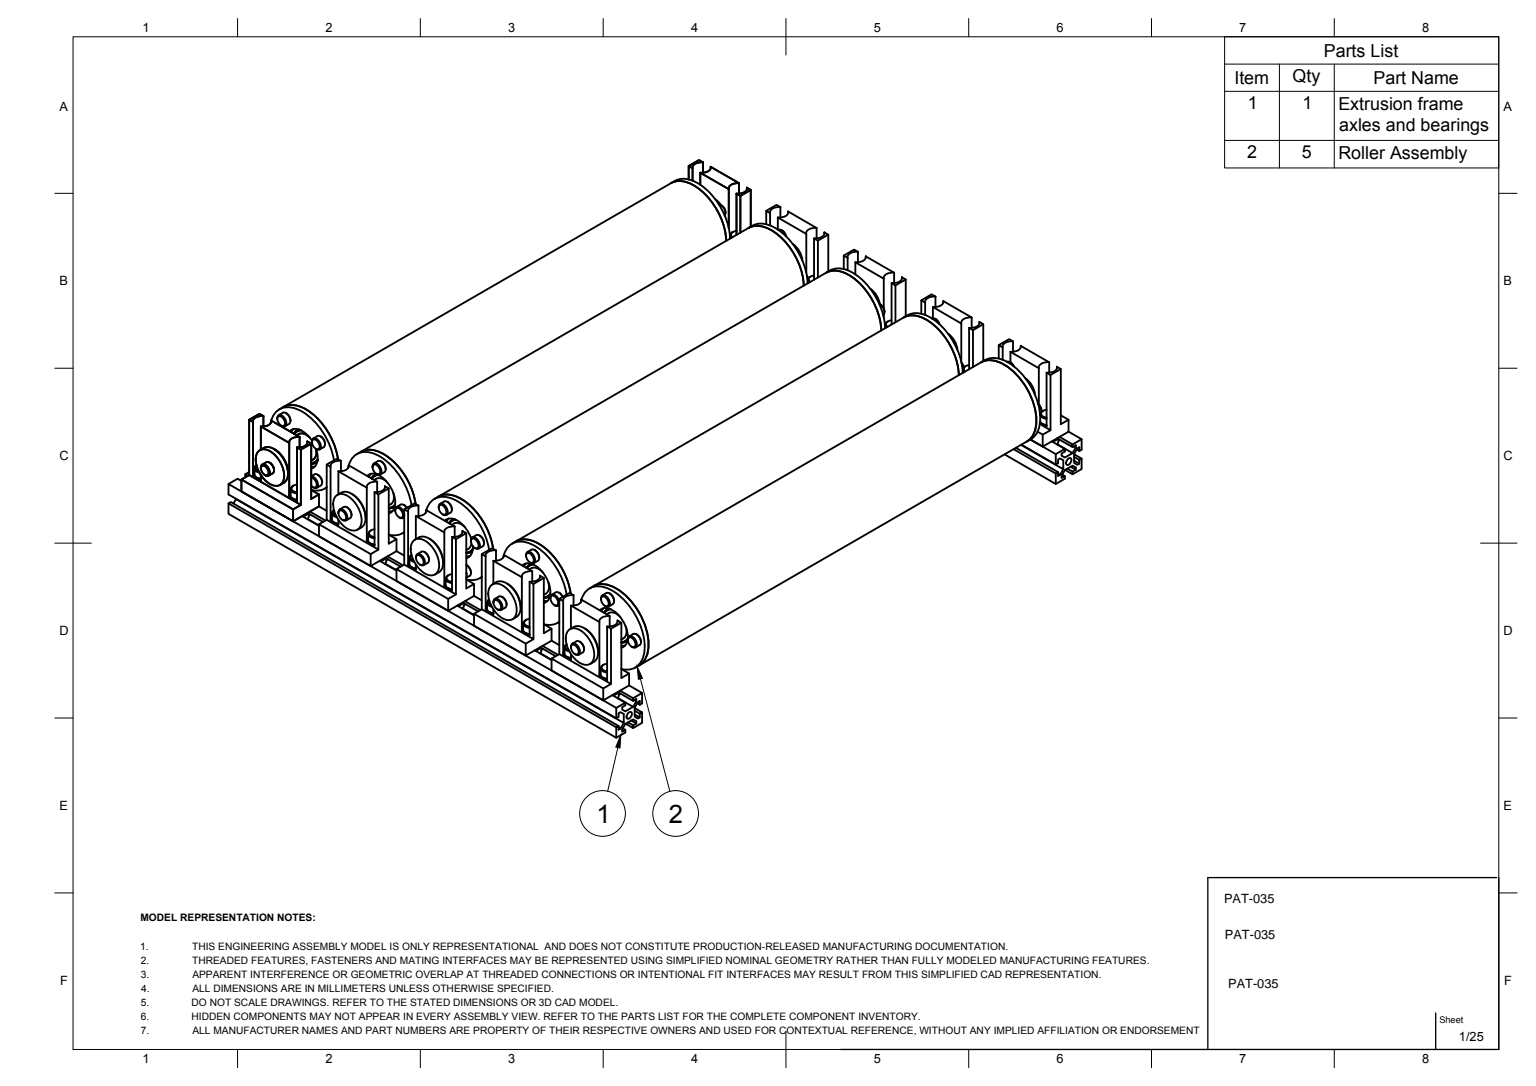
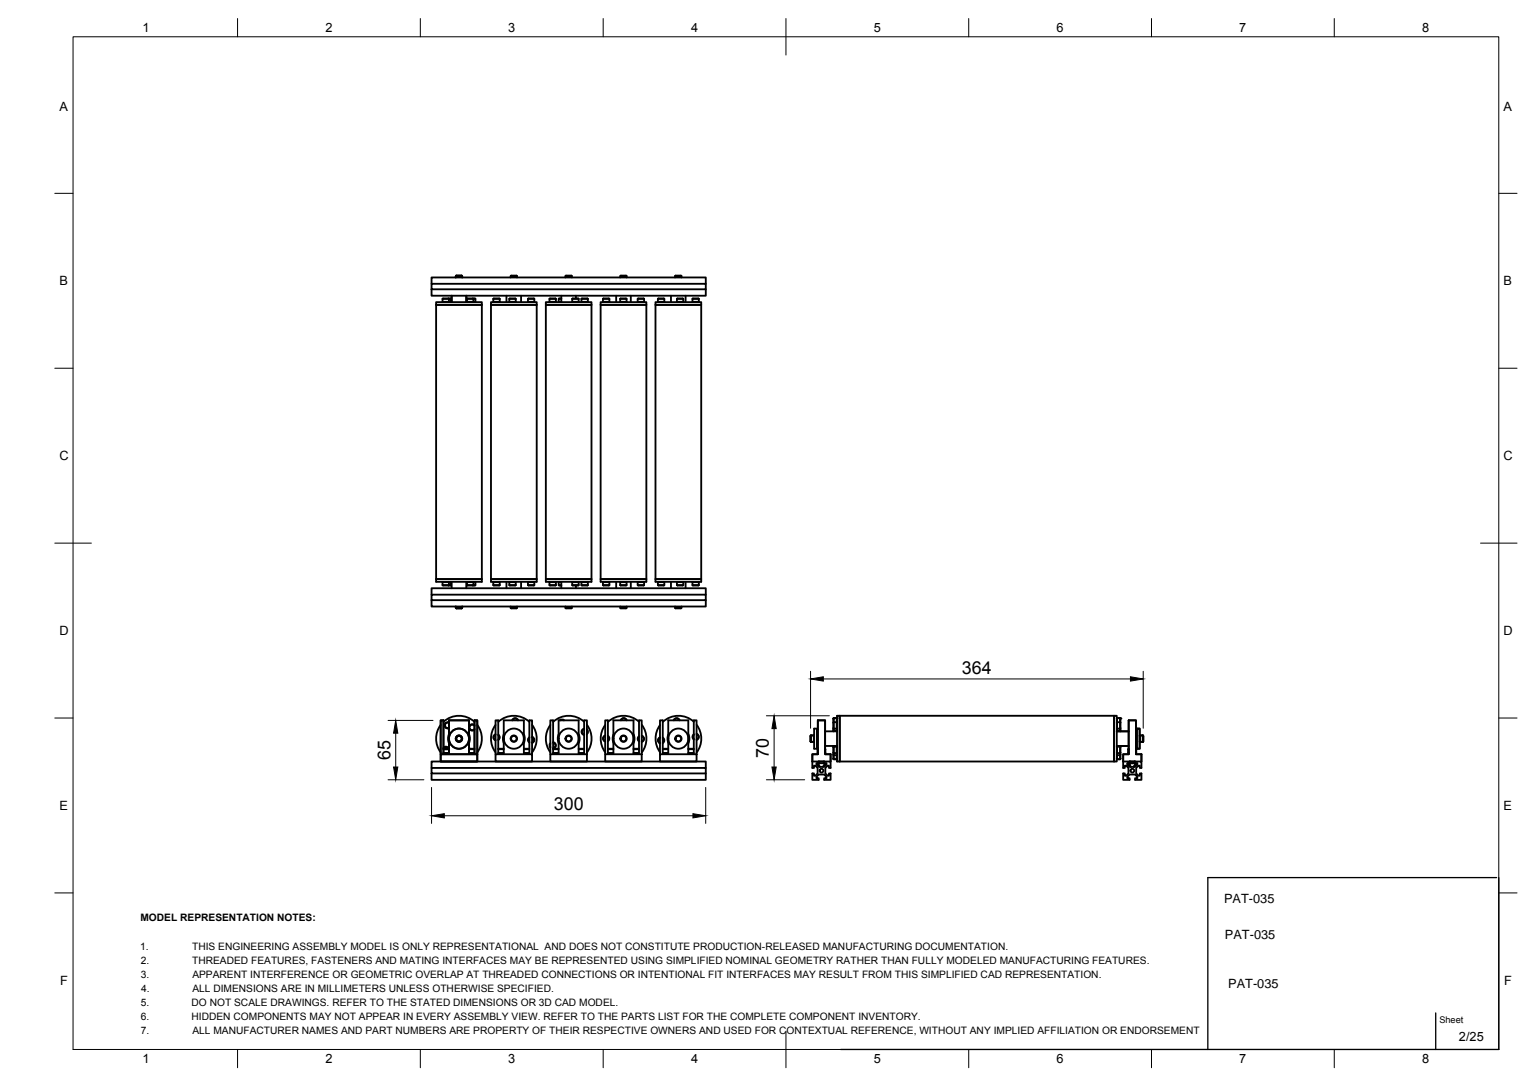
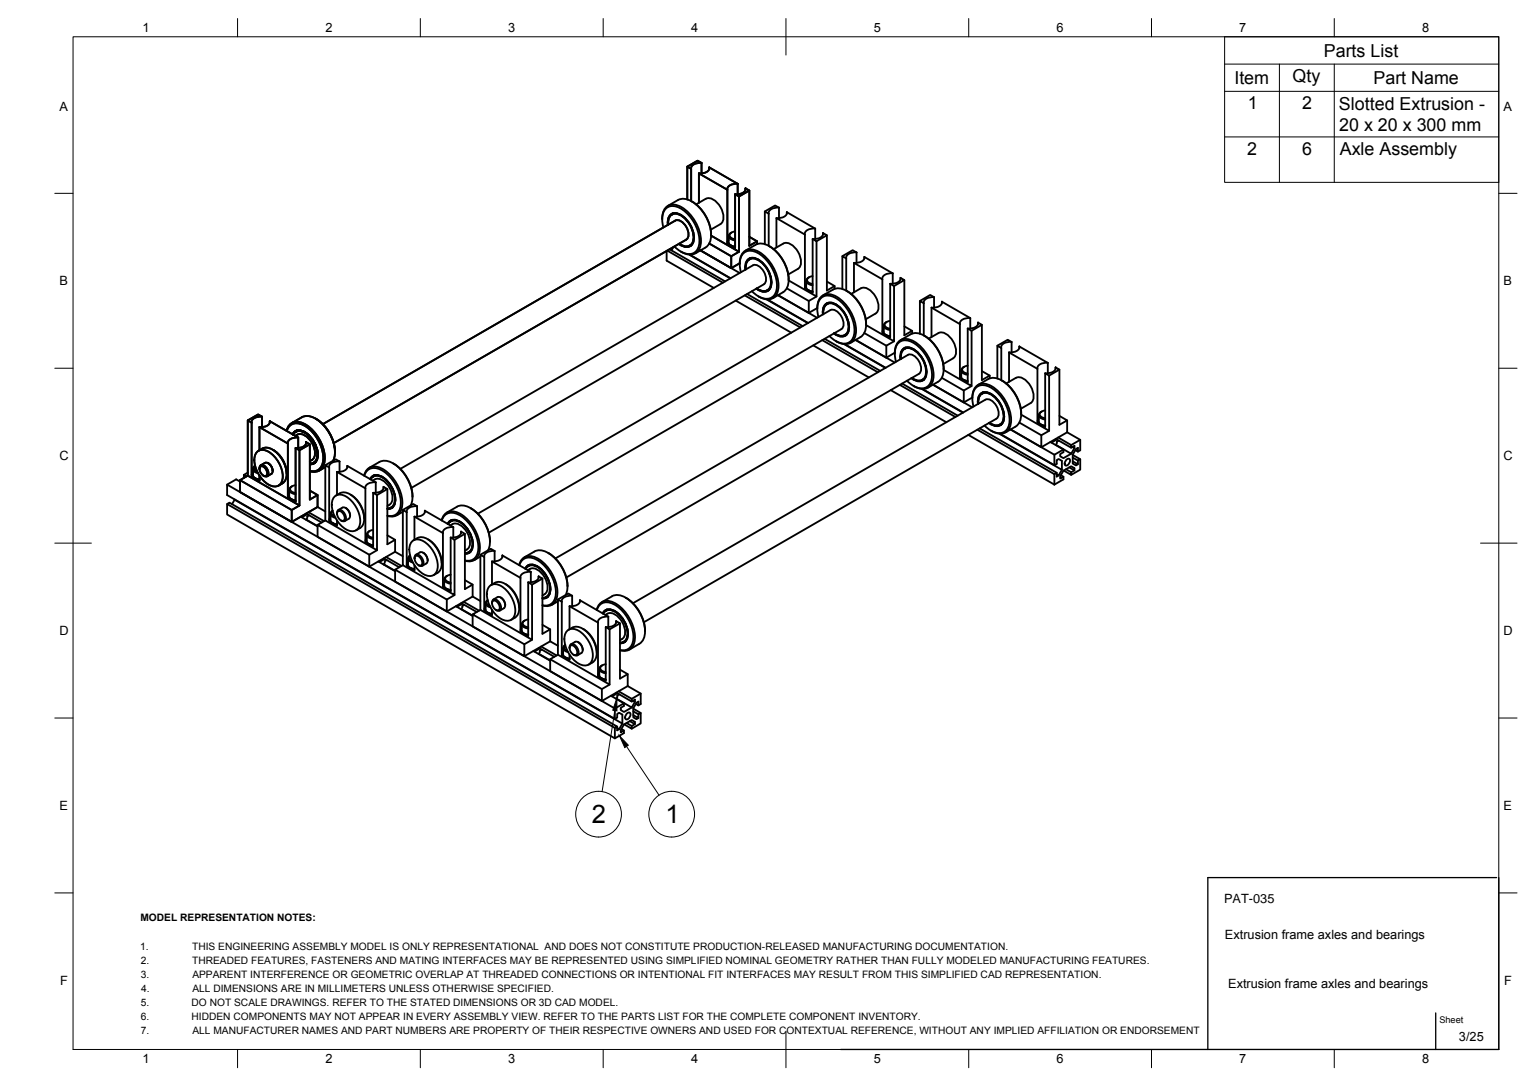
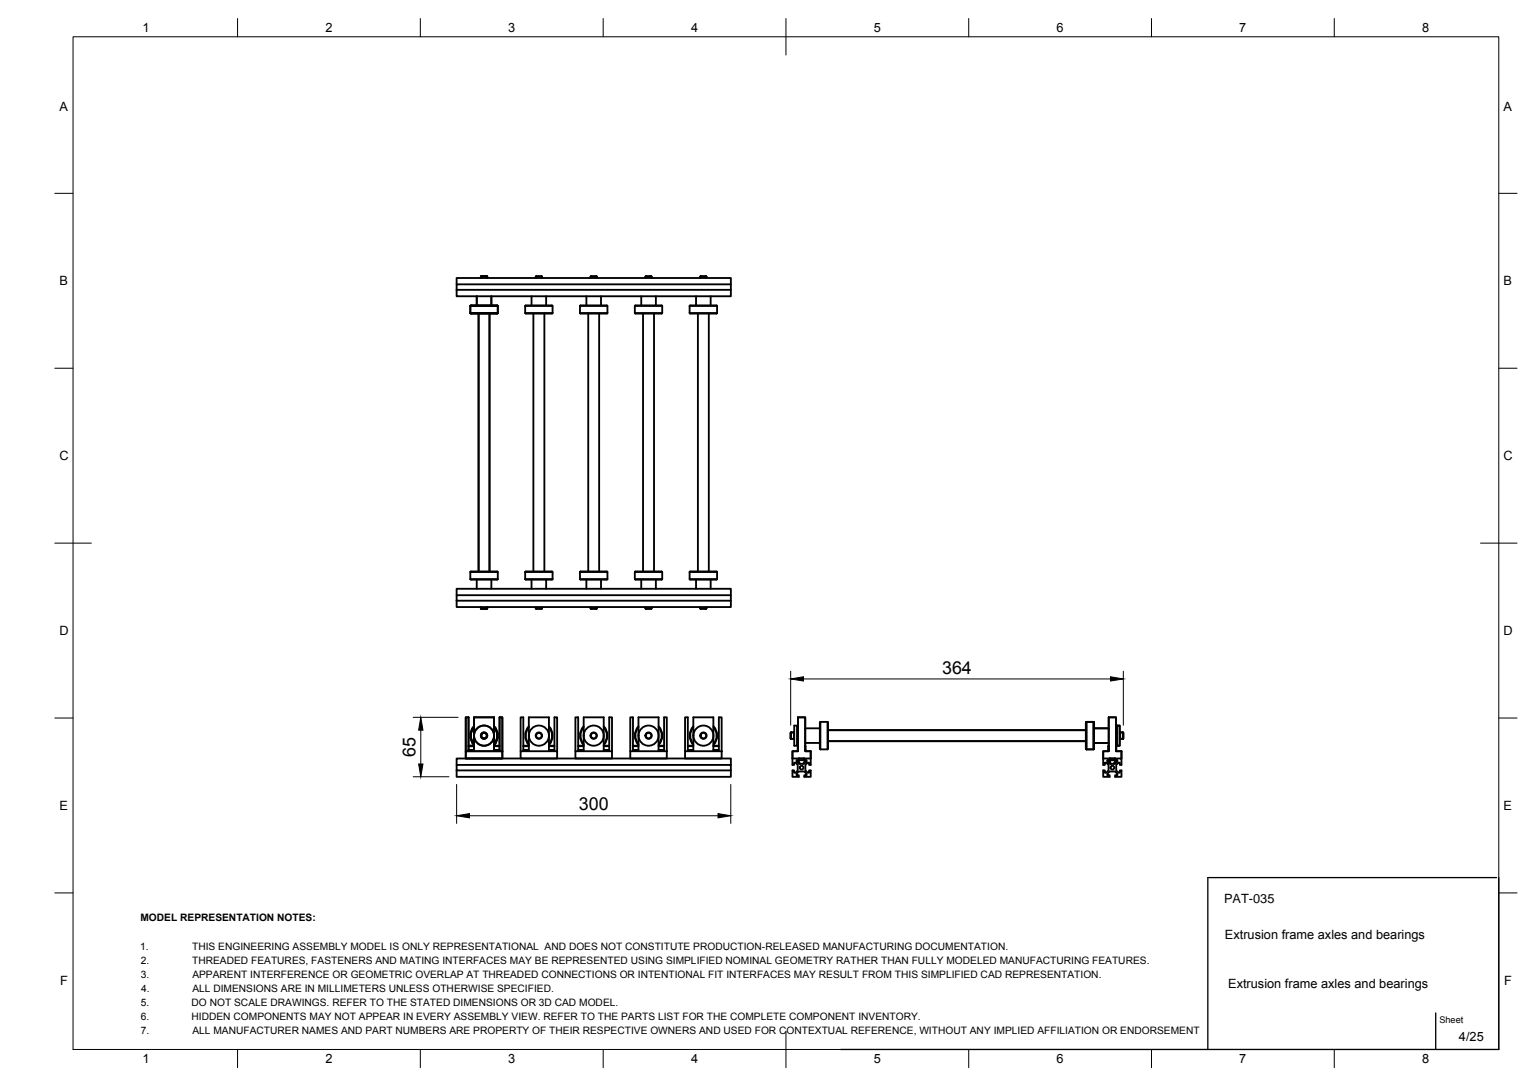
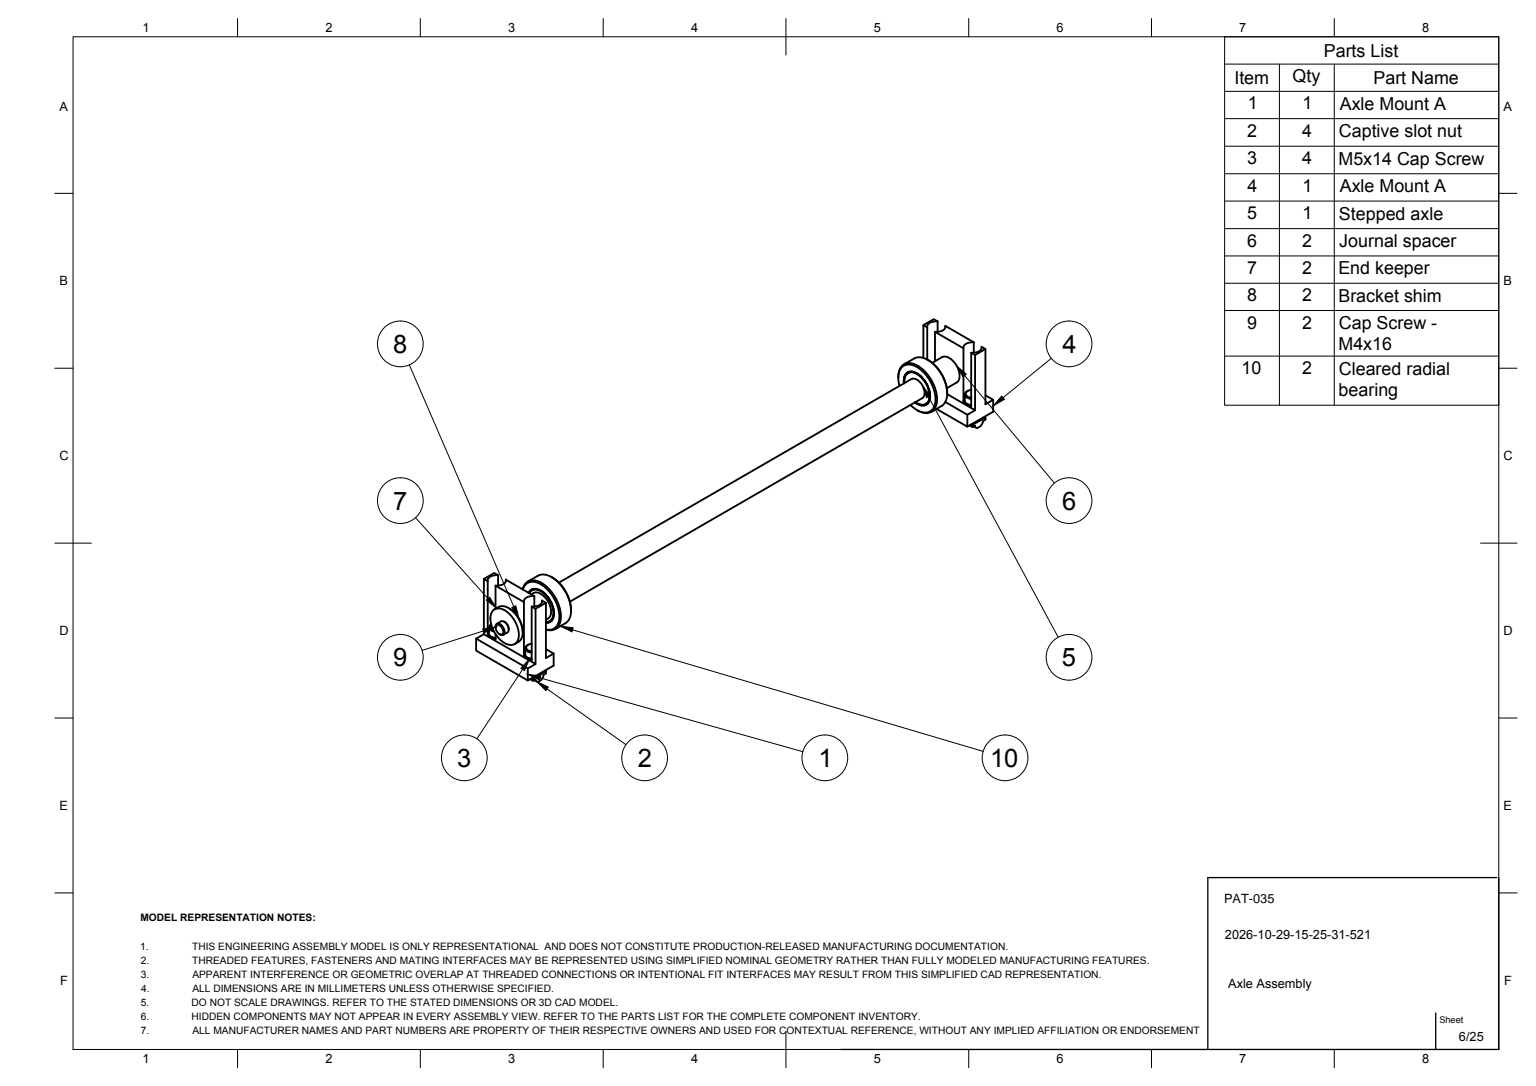
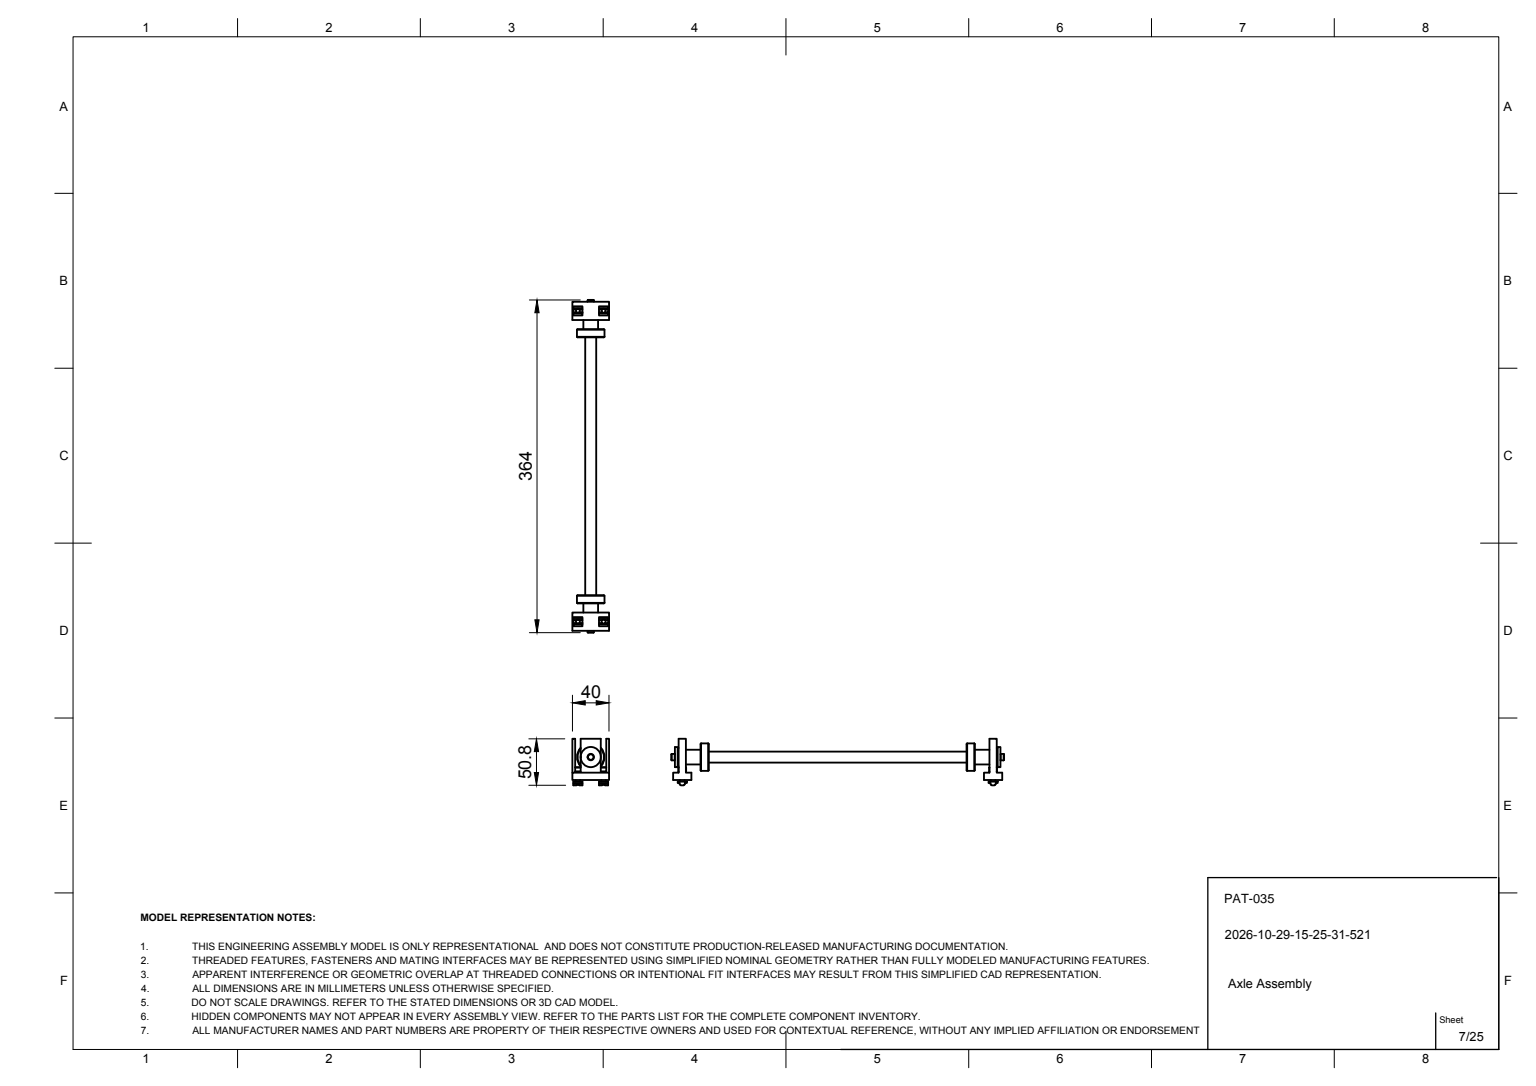
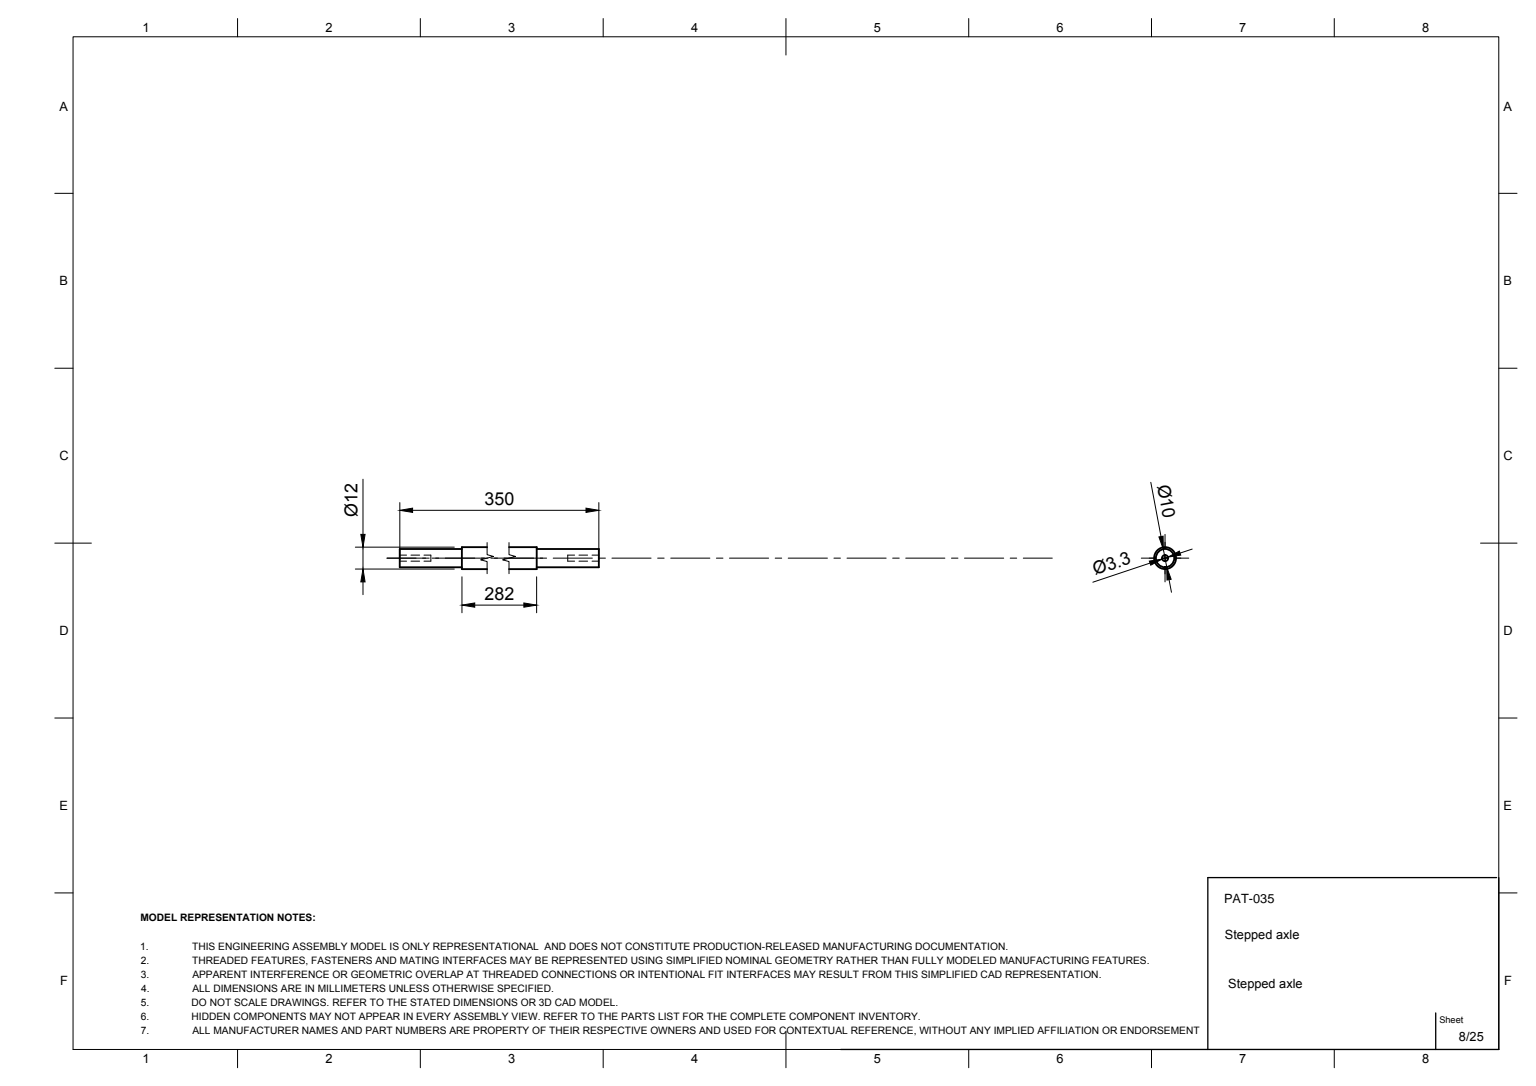
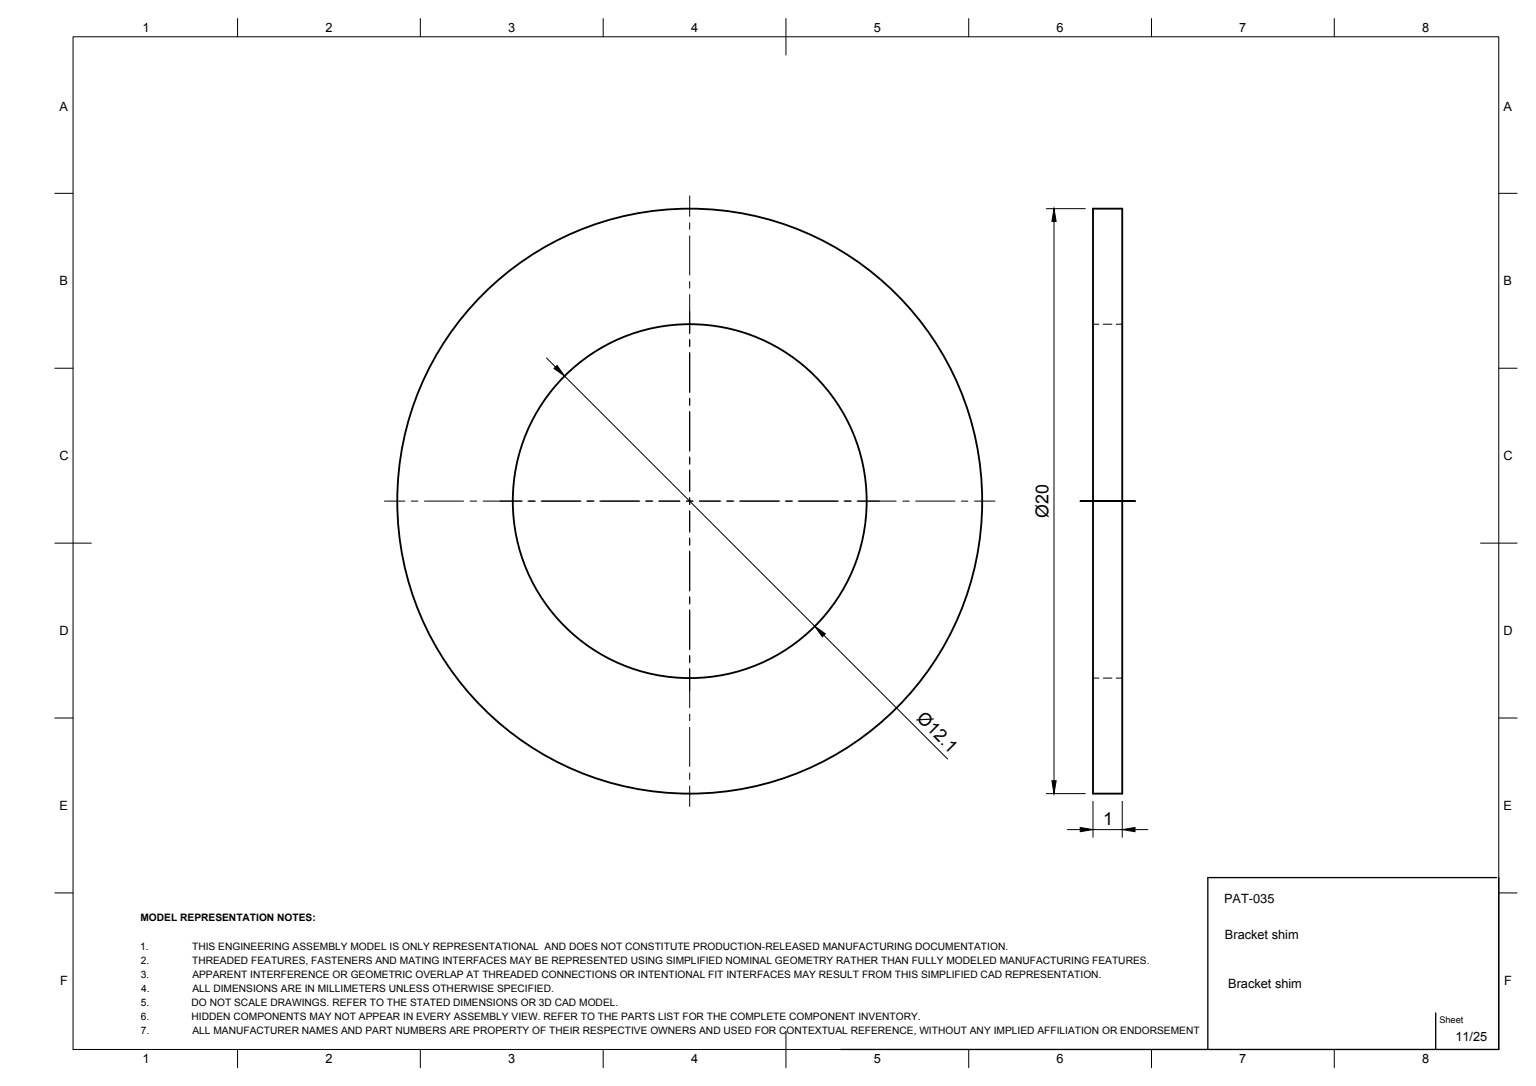
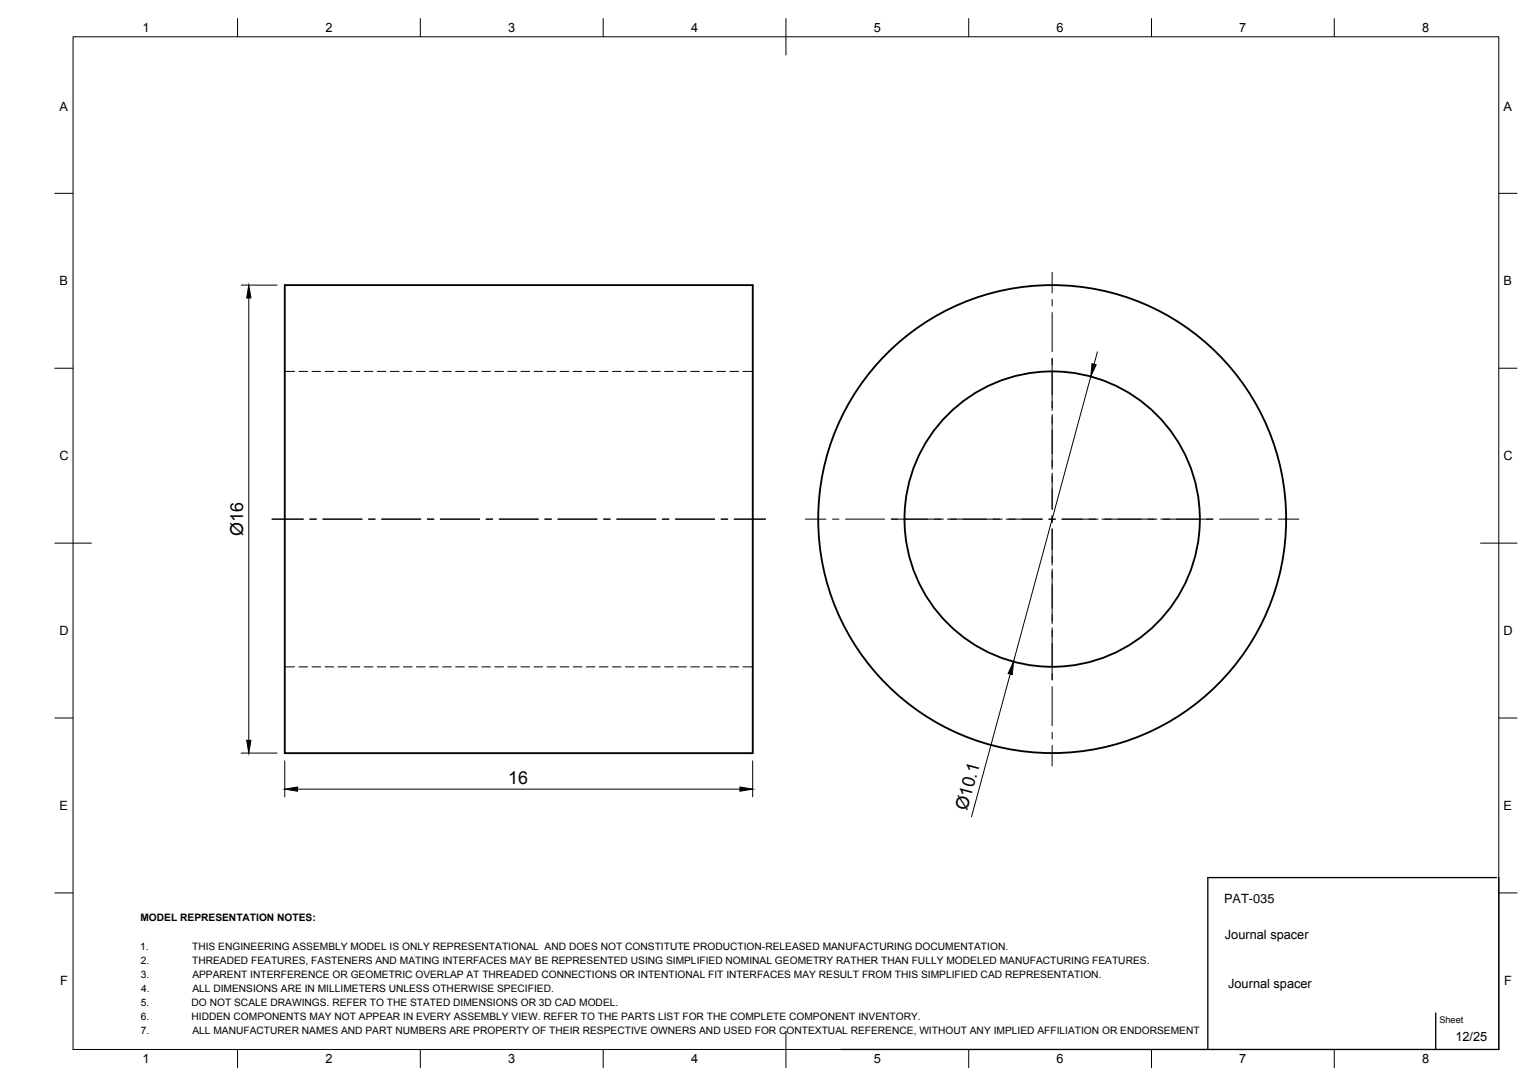
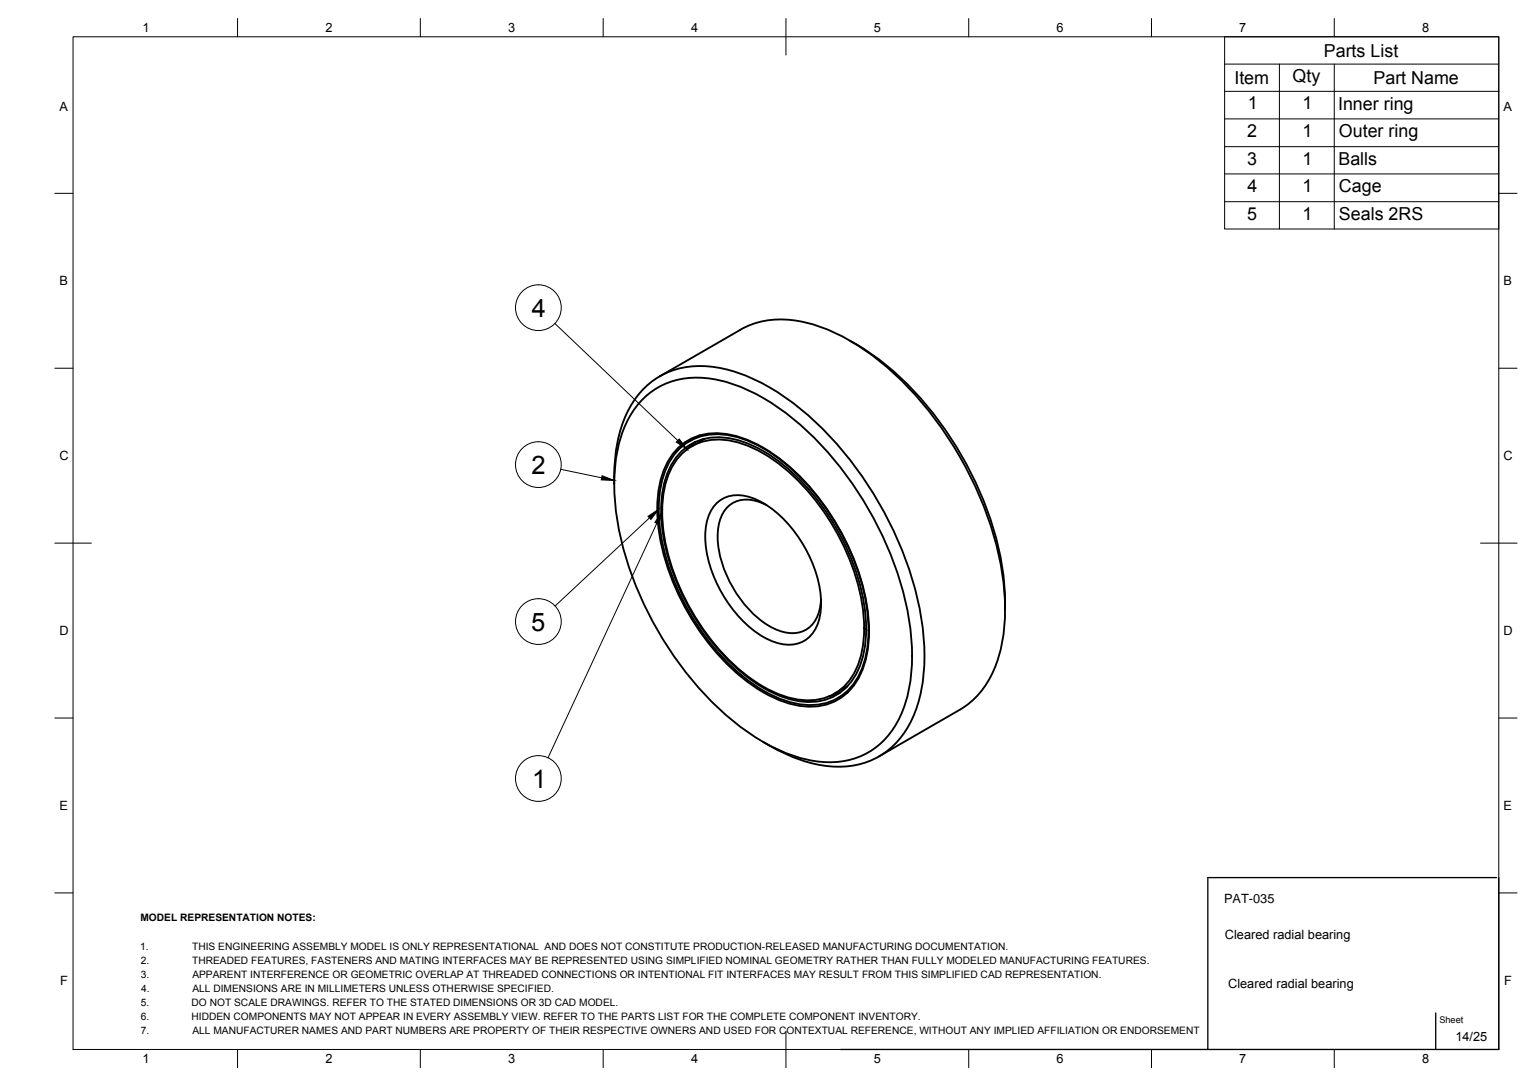
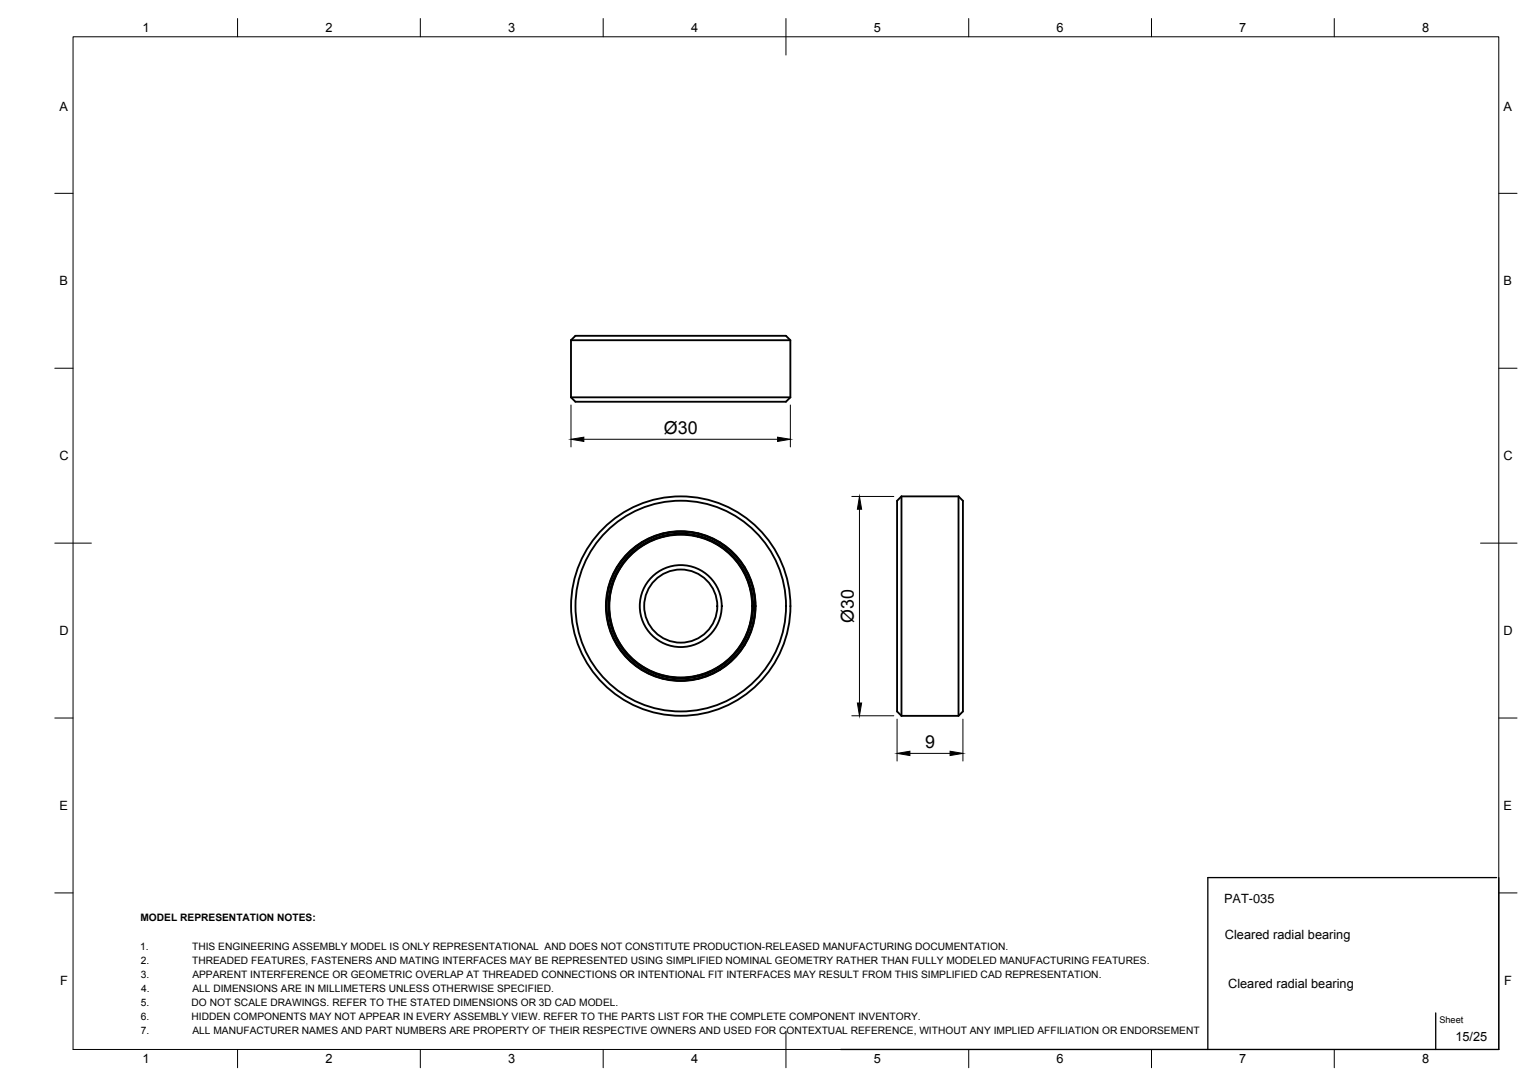
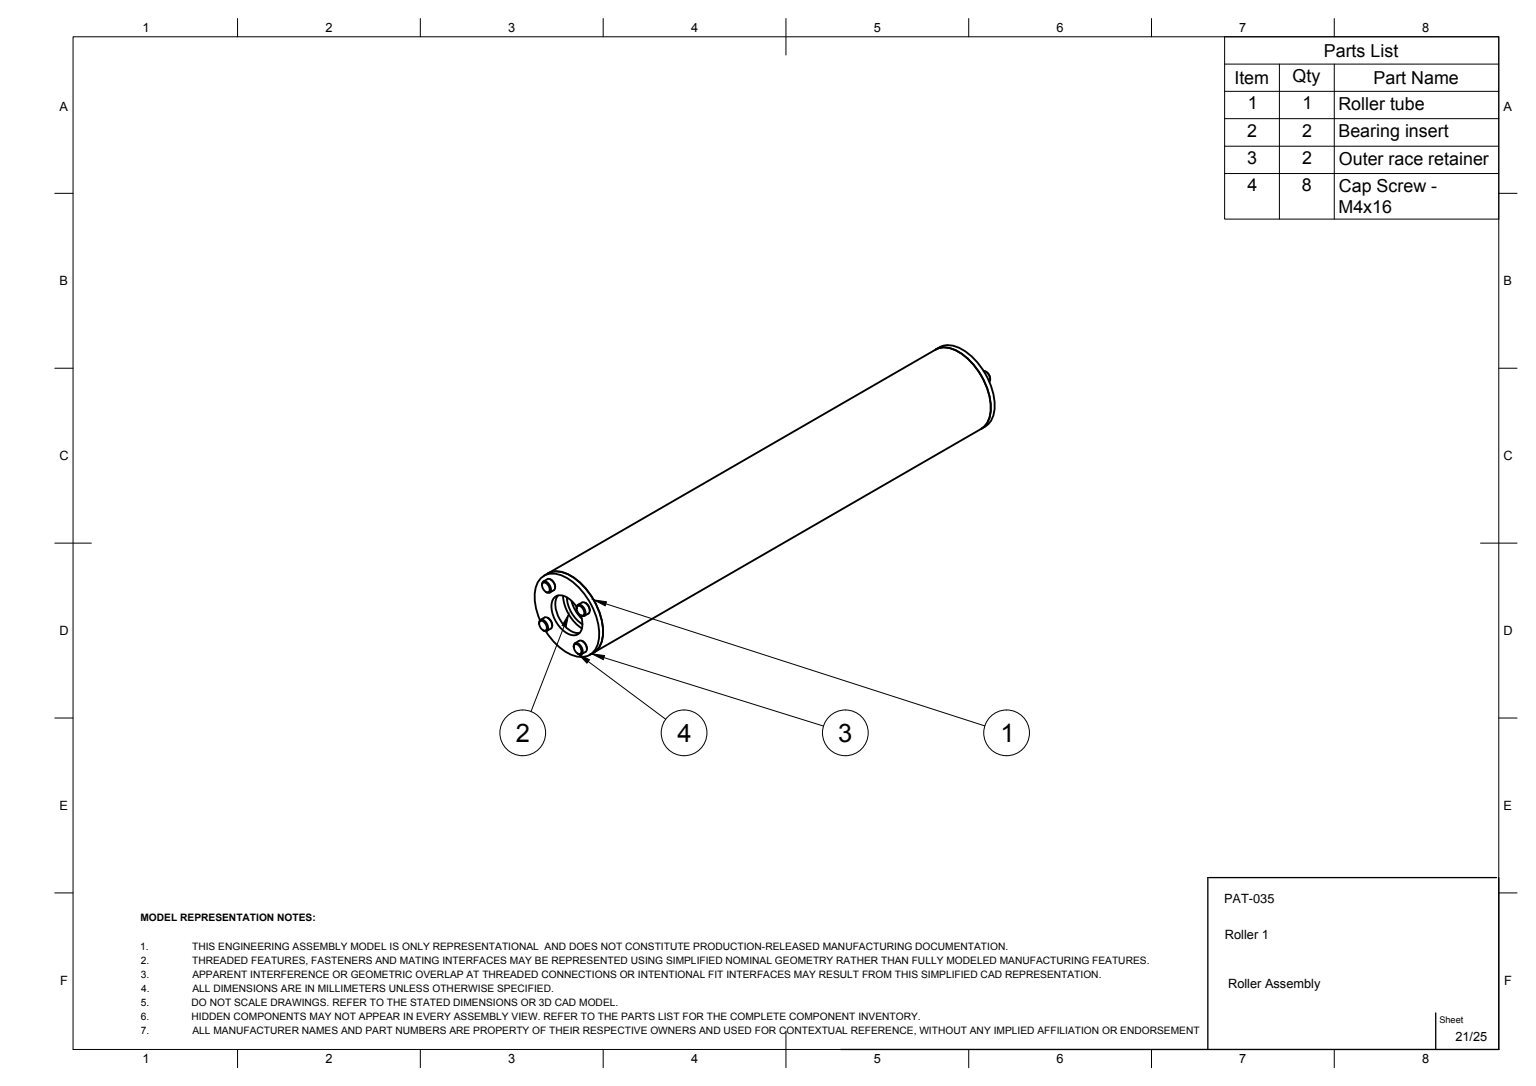
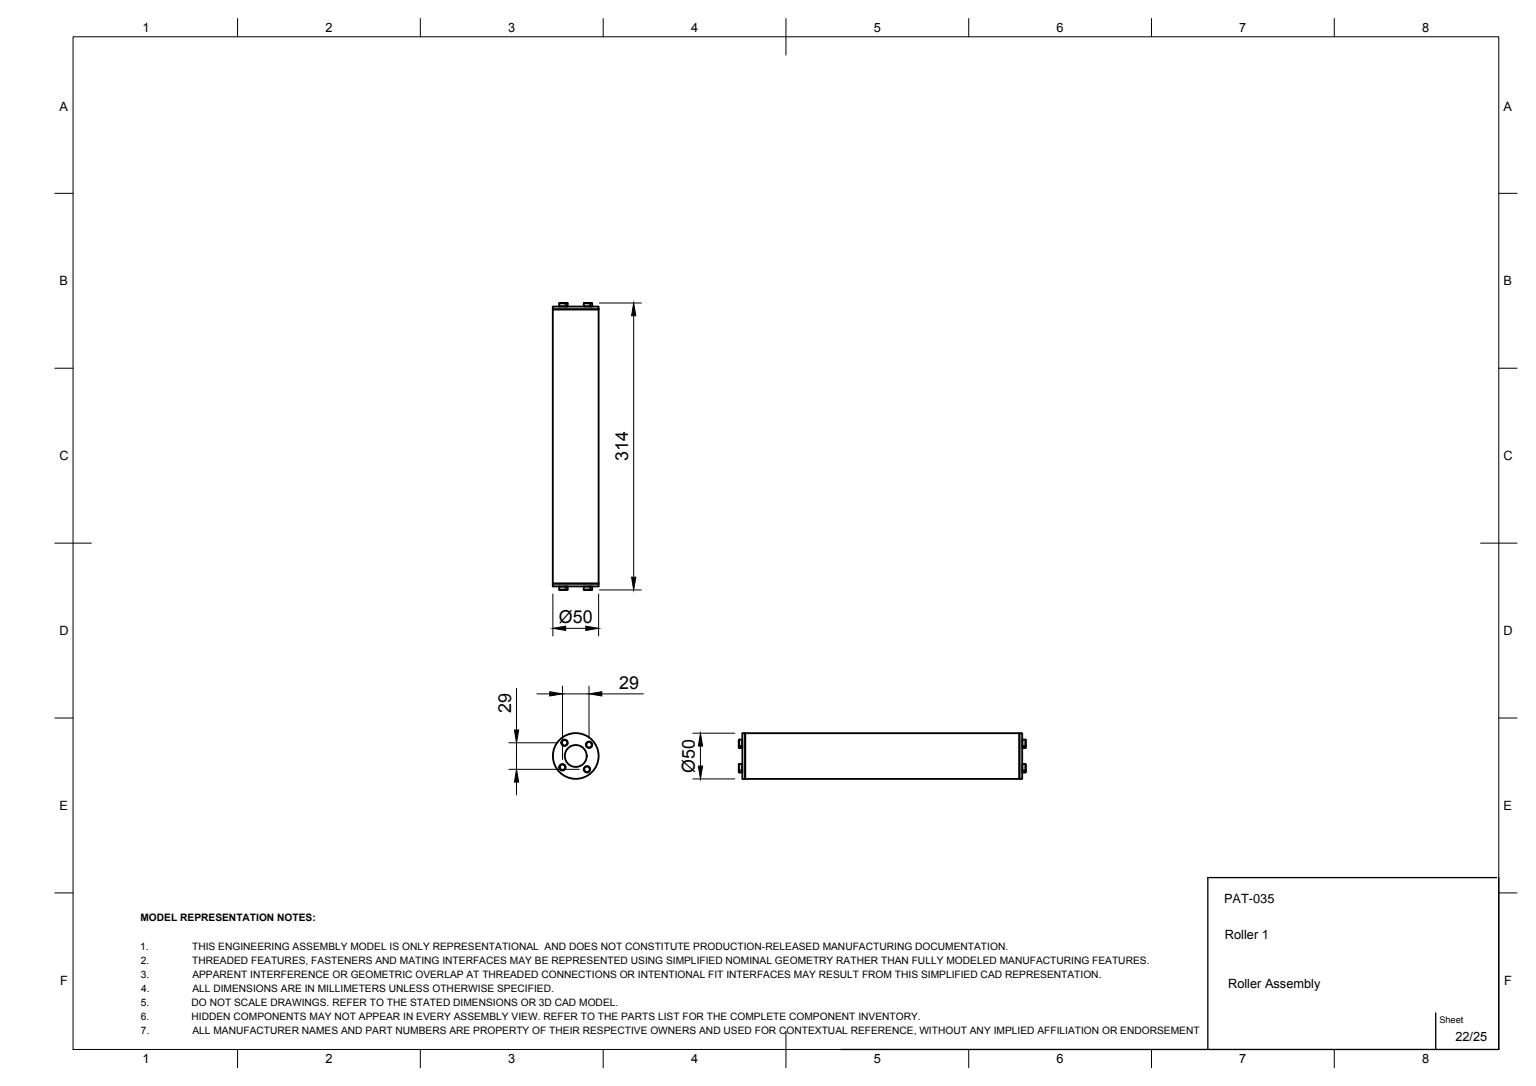
ISO-10303-21;
HEADER;
/* Generated by software containing ST-Developer
 * from STEP Tools, Inc. (www.steptools.com) 
 */

FILE_DESCRIPTION(
/* description */ ('Five-roller gravity conveyor'),
/* implementation_level */ '2;1');

FILE_NAME(
/* name */ 'PAT-035',
/* time_stamp */ '2026-10-29T15:36:43-07:00',
/* author */ (''),
/* organization */ (''),
/* preprocessor_version */ 'ST-DEVELOPER v20.2',
/* originating_system */ 'Autodesk Translation Framework v15.17.0.0',
/* authorisation */ '');

FILE_SCHEMA (('AUTOMOTIVE_DESIGN { 1 0 10303 214 3 1 1 }'));
ENDSEC;

DATA;
#10=MECHANICAL_DESIGN_GEOMETRIC_PRESENTATION_REPRESENTATION('',(#312,#313,
#314,#315,#316,#317,#318,#319,#320,#321,#322,#323,#324,#325,#326,#327,#328,
#329,#330,#331,#332,#333,#334,#335,#336,#337),#7806);
#11=ITEM_DEFINED_TRANSFORMATION($,$,#4619,#4747);
#12=ITEM_DEFINED_TRANSFORMATION($,$,#4639,#4748);
#13=ITEM_DEFINED_TRANSFORMATION($,$,#4659,#4749);
#14=ITEM_DEFINED_TRANSFORMATION($,$,#4676,#4750);
#15=ITEM_DEFINED_TRANSFORMATION($,$,#4730,#4751);
#16=ITEM_DEFINED_TRANSFORMATION($,$,#4479,#4861);
#17=ITEM_DEFINED_TRANSFORMATION($,$,#4501,#4862);
#18=ITEM_DEFINED_TRANSFORMATION($,$,#4597,#4863);
#19=ITEM_DEFINED_TRANSFORMATION($,$,#4597,#4864);
#20=ITEM_DEFINED_TRANSFORMATION($,$,#4573,#4865);
#21=ITEM_DEFINED_TRANSFORMATION($,$,#4537,#4866);
#22=ITEM_DEFINED_TRANSFORMATION($,$,#4573,#4867);
#23=ITEM_DEFINED_TRANSFORMATION($,$,#4618,#4868);
#24=ITEM_DEFINED_TRANSFORMATION($,$,#4835,#4869);
#25=ITEM_DEFINED_TRANSFORMATION($,$,#4770,#4870);
#26=ITEM_DEFINED_TRANSFORMATION($,$,#4573,#4871);
#27=ITEM_DEFINED_TRANSFORMATION($,$,#4597,#4872);
#28=ITEM_DEFINED_TRANSFORMATION($,$,#4573,#4873);
#29=ITEM_DEFINED_TRANSFORMATION($,$,#4597,#4874);
#30=ITEM_DEFINED_TRANSFORMATION($,$,#4761,#4875);
#31=ITEM_DEFINED_TRANSFORMATION($,$,#4752,#4876);
#32=ITEM_DEFINED_TRANSFORMATION($,$,#4618,#4877);
#33=ITEM_DEFINED_TRANSFORMATION($,$,#4752,#4878);
#34=ITEM_DEFINED_TRANSFORMATION($,$,#4761,#4879);
#35=ITEM_DEFINED_TRANSFORMATION($,$,#4835,#4880);
#36=ITEM_DEFINED_TRANSFORMATION($,$,#4770,#4881);
#37=ITEM_DEFINED_TRANSFORMATION($,$,#4428,#4882);
#38=ITEM_DEFINED_TRANSFORMATION($,$,#4428,#4883);
#39=ITEM_DEFINED_TRANSFORMATION($,$,#4478,#4884);
#40=ITEM_DEFINED_TRANSFORMATION($,$,#4478,#4885);
#41=ITEM_DEFINED_TRANSFORMATION($,$,#4478,#4886);
#42=ITEM_DEFINED_TRANSFORMATION($,$,#4478,#4887);
#43=ITEM_DEFINED_TRANSFORMATION($,$,#4478,#4888);
#44=ITEM_DEFINED_TRANSFORMATION($,$,#4478,#4889);
#45=ITEM_DEFINED_TRANSFORMATION($,$,#4780,#4890);
#46=ITEM_DEFINED_TRANSFORMATION($,$,#4789,#4891);
#47=ITEM_DEFINED_TRANSFORMATION($,$,#4789,#4892);
#48=ITEM_DEFINED_TRANSFORMATION($,$,#4814,#4893);
#49=ITEM_DEFINED_TRANSFORMATION($,$,#4814,#4894);
#50=ITEM_DEFINED_TRANSFORMATION($,$,#4835,#4895);
#51=ITEM_DEFINED_TRANSFORMATION($,$,#4835,#4896);
#52=ITEM_DEFINED_TRANSFORMATION($,$,#4835,#4897);
#53=ITEM_DEFINED_TRANSFORMATION($,$,#4835,#4898);
#54=ITEM_DEFINED_TRANSFORMATION($,$,#4835,#4899);
#55=ITEM_DEFINED_TRANSFORMATION($,$,#4835,#4900);
#56=ITEM_DEFINED_TRANSFORMATION($,$,#4835,#4901);
#57=ITEM_DEFINED_TRANSFORMATION($,$,#4835,#4902);
#58=ITEM_DEFINED_TRANSFORMATION($,$,#4427,#4903);
#59=ITEM_DEFINED_TRANSFORMATION($,$,#4779,#4904);
#60=ITEM_DEFINED_TRANSFORMATION($,$,#4779,#4905);
#61=ITEM_DEFINED_TRANSFORMATION($,$,#4779,#4906);
#62=ITEM_DEFINED_TRANSFORMATION($,$,#4779,#4907);
#63=ITEM_DEFINED_TRANSFORMATION($,$,#4779,#4908);
#64=(
REPRESENTATION_RELATIONSHIP($,$,#7920,#7919)
REPRESENTATION_RELATIONSHIP_WITH_TRANSFORMATION(#11)
SHAPE_REPRESENTATION_RELATIONSHIP()
);
#65=(
REPRESENTATION_RELATIONSHIP($,$,#7921,#7919)
REPRESENTATION_RELATIONSHIP_WITH_TRANSFORMATION(#12)
SHAPE_REPRESENTATION_RELATIONSHIP()
);
#66=(
REPRESENTATION_RELATIONSHIP($,$,#7922,#7919)
REPRESENTATION_RELATIONSHIP_WITH_TRANSFORMATION(#13)
SHAPE_REPRESENTATION_RELATIONSHIP()
);
#67=(
REPRESENTATION_RELATIONSHIP($,$,#7923,#7919)
REPRESENTATION_RELATIONSHIP_WITH_TRANSFORMATION(#14)
SHAPE_REPRESENTATION_RELATIONSHIP()
);
#68=(
REPRESENTATION_RELATIONSHIP($,$,#7924,#7919)
REPRESENTATION_RELATIONSHIP_WITH_TRANSFORMATION(#15)
SHAPE_REPRESENTATION_RELATIONSHIP()
);
#69=(
REPRESENTATION_RELATIONSHIP($,$,#7914,#7913)
REPRESENTATION_RELATIONSHIP_WITH_TRANSFORMATION(#16)
SHAPE_REPRESENTATION_RELATIONSHIP()
);
#70=(
REPRESENTATION_RELATIONSHIP($,$,#7915,#7913)
REPRESENTATION_RELATIONSHIP_WITH_TRANSFORMATION(#17)
SHAPE_REPRESENTATION_RELATIONSHIP()
);
#71=(
REPRESENTATION_RELATIONSHIP($,$,#7918,#7913)
REPRESENTATION_RELATIONSHIP_WITH_TRANSFORMATION(#18)
SHAPE_REPRESENTATION_RELATIONSHIP()
);
#72=(
REPRESENTATION_RELATIONSHIP($,$,#7918,#7913)
REPRESENTATION_RELATIONSHIP_WITH_TRANSFORMATION(#19)
SHAPE_REPRESENTATION_RELATIONSHIP()
);
#73=(
REPRESENTATION_RELATIONSHIP($,$,#7917,#7913)
REPRESENTATION_RELATIONSHIP_WITH_TRANSFORMATION(#20)
SHAPE_REPRESENTATION_RELATIONSHIP()
);
#74=(
REPRESENTATION_RELATIONSHIP($,$,#7916,#7913)
REPRESENTATION_RELATIONSHIP_WITH_TRANSFORMATION(#21)
SHAPE_REPRESENTATION_RELATIONSHIP()
);
#75=(
REPRESENTATION_RELATIONSHIP($,$,#7917,#7913)
REPRESENTATION_RELATIONSHIP_WITH_TRANSFORMATION(#22)
SHAPE_REPRESENTATION_RELATIONSHIP()
);
#76=(
REPRESENTATION_RELATIONSHIP($,$,#7919,#7913)
REPRESENTATION_RELATIONSHIP_WITH_TRANSFORMATION(#23)
SHAPE_REPRESENTATION_RELATIONSHIP()
);
#77=(
REPRESENTATION_RELATIONSHIP($,$,#7932,#7913)
REPRESENTATION_RELATIONSHIP_WITH_TRANSFORMATION(#24)
SHAPE_REPRESENTATION_RELATIONSHIP()
);
#78=(
REPRESENTATION_RELATIONSHIP($,$,#7927,#7913)
REPRESENTATION_RELATIONSHIP_WITH_TRANSFORMATION(#25)
SHAPE_REPRESENTATION_RELATIONSHIP()
);
#79=(
REPRESENTATION_RELATIONSHIP($,$,#7917,#7913)
REPRESENTATION_RELATIONSHIP_WITH_TRANSFORMATION(#26)
SHAPE_REPRESENTATION_RELATIONSHIP()
);
#80=(
REPRESENTATION_RELATIONSHIP($,$,#7918,#7913)
REPRESENTATION_RELATIONSHIP_WITH_TRANSFORMATION(#27)
SHAPE_REPRESENTATION_RELATIONSHIP()
);
#81=(
REPRESENTATION_RELATIONSHIP($,$,#7917,#7913)
REPRESENTATION_RELATIONSHIP_WITH_TRANSFORMATION(#28)
SHAPE_REPRESENTATION_RELATIONSHIP()
);
#82=(
REPRESENTATION_RELATIONSHIP($,$,#7918,#7913)
REPRESENTATION_RELATIONSHIP_WITH_TRANSFORMATION(#29)
SHAPE_REPRESENTATION_RELATIONSHIP()
);
#83=(
REPRESENTATION_RELATIONSHIP($,$,#7926,#7913)
REPRESENTATION_RELATIONSHIP_WITH_TRANSFORMATION(#30)
SHAPE_REPRESENTATION_RELATIONSHIP()
);
#84=(
REPRESENTATION_RELATIONSHIP($,$,#7925,#7913)
REPRESENTATION_RELATIONSHIP_WITH_TRANSFORMATION(#31)
SHAPE_REPRESENTATION_RELATIONSHIP()
);
#85=(
REPRESENTATION_RELATIONSHIP($,$,#7919,#7913)
REPRESENTATION_RELATIONSHIP_WITH_TRANSFORMATION(#32)
SHAPE_REPRESENTATION_RELATIONSHIP()
);
#86=(
REPRESENTATION_RELATIONSHIP($,$,#7925,#7913)
REPRESENTATION_RELATIONSHIP_WITH_TRANSFORMATION(#33)
SHAPE_REPRESENTATION_RELATIONSHIP()
);
#87=(
REPRESENTATION_RELATIONSHIP($,$,#7926,#7913)
REPRESENTATION_RELATIONSHIP_WITH_TRANSFORMATION(#34)
SHAPE_REPRESENTATION_RELATIONSHIP()
);
#88=(
REPRESENTATION_RELATIONSHIP($,$,#7932,#7913)
REPRESENTATION_RELATIONSHIP_WITH_TRANSFORMATION(#35)
SHAPE_REPRESENTATION_RELATIONSHIP()
);
#89=(
REPRESENTATION_RELATIONSHIP($,$,#7927,#7913)
REPRESENTATION_RELATIONSHIP_WITH_TRANSFORMATION(#36)
SHAPE_REPRESENTATION_RELATIONSHIP()
);
#90=(
REPRESENTATION_RELATIONSHIP($,$,#7912,#7911)
REPRESENTATION_RELATIONSHIP_WITH_TRANSFORMATION(#37)
SHAPE_REPRESENTATION_RELATIONSHIP()
);
#91=(
REPRESENTATION_RELATIONSHIP($,$,#7912,#7911)
REPRESENTATION_RELATIONSHIP_WITH_TRANSFORMATION(#38)
SHAPE_REPRESENTATION_RELATIONSHIP()
);
#92=(
REPRESENTATION_RELATIONSHIP($,$,#7913,#7911)
REPRESENTATION_RELATIONSHIP_WITH_TRANSFORMATION(#39)
SHAPE_REPRESENTATION_RELATIONSHIP()
);
#93=(
REPRESENTATION_RELATIONSHIP($,$,#7913,#7911)
REPRESENTATION_RELATIONSHIP_WITH_TRANSFORMATION(#40)
SHAPE_REPRESENTATION_RELATIONSHIP()
);
#94=(
REPRESENTATION_RELATIONSHIP($,$,#7913,#7911)
REPRESENTATION_RELATIONSHIP_WITH_TRANSFORMATION(#41)
SHAPE_REPRESENTATION_RELATIONSHIP()
);
#95=(
REPRESENTATION_RELATIONSHIP($,$,#7913,#7911)
REPRESENTATION_RELATIONSHIP_WITH_TRANSFORMATION(#42)
SHAPE_REPRESENTATION_RELATIONSHIP()
);
#96=(
REPRESENTATION_RELATIONSHIP($,$,#7913,#7911)
REPRESENTATION_RELATIONSHIP_WITH_TRANSFORMATION(#43)
SHAPE_REPRESENTATION_RELATIONSHIP()
);
#97=(
REPRESENTATION_RELATIONSHIP($,$,#7913,#7911)
REPRESENTATION_RELATIONSHIP_WITH_TRANSFORMATION(#44)
SHAPE_REPRESENTATION_RELATIONSHIP()
);
#98=(
REPRESENTATION_RELATIONSHIP($,$,#7929,#7928)
REPRESENTATION_RELATIONSHIP_WITH_TRANSFORMATION(#45)
SHAPE_REPRESENTATION_RELATIONSHIP()
);
#99=(
REPRESENTATION_RELATIONSHIP($,$,#7930,#7928)
REPRESENTATION_RELATIONSHIP_WITH_TRANSFORMATION(#46)
SHAPE_REPRESENTATION_RELATIONSHIP()
);
#100=(
REPRESENTATION_RELATIONSHIP($,$,#7930,#7928)
REPRESENTATION_RELATIONSHIP_WITH_TRANSFORMATION(#47)
SHAPE_REPRESENTATION_RELATIONSHIP()
);
#101=(
REPRESENTATION_RELATIONSHIP($,$,#7931,#7928)
REPRESENTATION_RELATIONSHIP_WITH_TRANSFORMATION(#48)
SHAPE_REPRESENTATION_RELATIONSHIP()
);
#102=(
REPRESENTATION_RELATIONSHIP($,$,#7931,#7928)
REPRESENTATION_RELATIONSHIP_WITH_TRANSFORMATION(#49)
SHAPE_REPRESENTATION_RELATIONSHIP()
);
#103=(
REPRESENTATION_RELATIONSHIP($,$,#7932,#7928)
REPRESENTATION_RELATIONSHIP_WITH_TRANSFORMATION(#50)
SHAPE_REPRESENTATION_RELATIONSHIP()
);
#104=(
REPRESENTATION_RELATIONSHIP($,$,#7932,#7928)
REPRESENTATION_RELATIONSHIP_WITH_TRANSFORMATION(#51)
SHAPE_REPRESENTATION_RELATIONSHIP()
);
#105=(
REPRESENTATION_RELATIONSHIP($,$,#7932,#7928)
REPRESENTATION_RELATIONSHIP_WITH_TRANSFORMATION(#52)
SHAPE_REPRESENTATION_RELATIONSHIP()
);
#106=(
REPRESENTATION_RELATIONSHIP($,$,#7932,#7928)
REPRESENTATION_RELATIONSHIP_WITH_TRANSFORMATION(#53)
SHAPE_REPRESENTATION_RELATIONSHIP()
);
#107=(
REPRESENTATION_RELATIONSHIP($,$,#7932,#7928)
REPRESENTATION_RELATIONSHIP_WITH_TRANSFORMATION(#54)
SHAPE_REPRESENTATION_RELATIONSHIP()
);
#108=(
REPRESENTATION_RELATIONSHIP($,$,#7932,#7928)
REPRESENTATION_RELATIONSHIP_WITH_TRANSFORMATION(#55)
SHAPE_REPRESENTATION_RELATIONSHIP()
);
#109=(
REPRESENTATION_RELATIONSHIP($,$,#7932,#7928)
REPRESENTATION_RELATIONSHIP_WITH_TRANSFORMATION(#56)
SHAPE_REPRESENTATION_RELATIONSHIP()
);
#110=(
REPRESENTATION_RELATIONSHIP($,$,#7932,#7928)
REPRESENTATION_RELATIONSHIP_WITH_TRANSFORMATION(#57)
SHAPE_REPRESENTATION_RELATIONSHIP()
);
#111=(
REPRESENTATION_RELATIONSHIP($,$,#7911,#7910)
REPRESENTATION_RELATIONSHIP_WITH_TRANSFORMATION(#58)
SHAPE_REPRESENTATION_RELATIONSHIP()
);
#112=(
REPRESENTATION_RELATIONSHIP($,$,#7928,#7910)
REPRESENTATION_RELATIONSHIP_WITH_TRANSFORMATION(#59)
SHAPE_REPRESENTATION_RELATIONSHIP()
);
#113=(
REPRESENTATION_RELATIONSHIP($,$,#7928,#7910)
REPRESENTATION_RELATIONSHIP_WITH_TRANSFORMATION(#60)
SHAPE_REPRESENTATION_RELATIONSHIP()
);
#114=(
REPRESENTATION_RELATIONSHIP($,$,#7928,#7910)
REPRESENTATION_RELATIONSHIP_WITH_TRANSFORMATION(#61)
SHAPE_REPRESENTATION_RELATIONSHIP()
);
#115=(
REPRESENTATION_RELATIONSHIP($,$,#7928,#7910)
REPRESENTATION_RELATIONSHIP_WITH_TRANSFORMATION(#62)
SHAPE_REPRESENTATION_RELATIONSHIP()
);
#116=(
REPRESENTATION_RELATIONSHIP($,$,#7928,#7910)
REPRESENTATION_RELATIONSHIP_WITH_TRANSFORMATION(#63)
SHAPE_REPRESENTATION_RELATIONSHIP()
);
#117=CONTEXT_DEPENDENT_SHAPE_REPRESENTATION(#64,#7849);
#118=CONTEXT_DEPENDENT_SHAPE_REPRESENTATION(#65,#7850);
#119=CONTEXT_DEPENDENT_SHAPE_REPRESENTATION(#66,#7851);
#120=CONTEXT_DEPENDENT_SHAPE_REPRESENTATION(#67,#7852);
#121=CONTEXT_DEPENDENT_SHAPE_REPRESENTATION(#68,#7853);
#122=CONTEXT_DEPENDENT_SHAPE_REPRESENTATION(#69,#7862);
#123=CONTEXT_DEPENDENT_SHAPE_REPRESENTATION(#70,#7863);
#124=CONTEXT_DEPENDENT_SHAPE_REPRESENTATION(#71,#7864);
#125=CONTEXT_DEPENDENT_SHAPE_REPRESENTATION(#72,#7865);
#126=CONTEXT_DEPENDENT_SHAPE_REPRESENTATION(#73,#7866);
#127=CONTEXT_DEPENDENT_SHAPE_REPRESENTATION(#74,#7867);
#128=CONTEXT_DEPENDENT_SHAPE_REPRESENTATION(#75,#7868);
#129=CONTEXT_DEPENDENT_SHAPE_REPRESENTATION(#76,#7869);
#130=CONTEXT_DEPENDENT_SHAPE_REPRESENTATION(#77,#7870);
#131=CONTEXT_DEPENDENT_SHAPE_REPRESENTATION(#78,#7871);
#132=CONTEXT_DEPENDENT_SHAPE_REPRESENTATION(#79,#7872);
#133=CONTEXT_DEPENDENT_SHAPE_REPRESENTATION(#80,#7873);
#134=CONTEXT_DEPENDENT_SHAPE_REPRESENTATION(#81,#7874);
#135=CONTEXT_DEPENDENT_SHAPE_REPRESENTATION(#82,#7875);
#136=CONTEXT_DEPENDENT_SHAPE_REPRESENTATION(#83,#7876);
#137=CONTEXT_DEPENDENT_SHAPE_REPRESENTATION(#84,#7877);
#138=CONTEXT_DEPENDENT_SHAPE_REPRESENTATION(#85,#7878);
#139=CONTEXT_DEPENDENT_SHAPE_REPRESENTATION(#86,#7879);
#140=CONTEXT_DEPENDENT_SHAPE_REPRESENTATION(#87,#7880);
#141=CONTEXT_DEPENDENT_SHAPE_REPRESENTATION(#88,#7881);
#142=CONTEXT_DEPENDENT_SHAPE_REPRESENTATION(#89,#7882);
#143=CONTEXT_DEPENDENT_SHAPE_REPRESENTATION(#90,#7883);
#144=CONTEXT_DEPENDENT_SHAPE_REPRESENTATION(#91,#7884);
#145=CONTEXT_DEPENDENT_SHAPE_REPRESENTATION(#92,#7885);
#146=CONTEXT_DEPENDENT_SHAPE_REPRESENTATION(#93,#7886);
#147=CONTEXT_DEPENDENT_SHAPE_REPRESENTATION(#94,#7887);
#148=CONTEXT_DEPENDENT_SHAPE_REPRESENTATION(#95,#7888);
#149=CONTEXT_DEPENDENT_SHAPE_REPRESENTATION(#96,#7889);
#150=CONTEXT_DEPENDENT_SHAPE_REPRESENTATION(#97,#7890);
#151=CONTEXT_DEPENDENT_SHAPE_REPRESENTATION(#98,#7891);
#152=CONTEXT_DEPENDENT_SHAPE_REPRESENTATION(#99,#7892);
#153=CONTEXT_DEPENDENT_SHAPE_REPRESENTATION(#100,#7893);
#154=CONTEXT_DEPENDENT_SHAPE_REPRESENTATION(#101,#7894);
#155=CONTEXT_DEPENDENT_SHAPE_REPRESENTATION(#102,#7895);
#156=CONTEXT_DEPENDENT_SHAPE_REPRESENTATION(#103,#7896);
#157=CONTEXT_DEPENDENT_SHAPE_REPRESENTATION(#104,#7897);
#158=CONTEXT_DEPENDENT_SHAPE_REPRESENTATION(#105,#7898);
#159=CONTEXT_DEPENDENT_SHAPE_REPRESENTATION(#106,#7899);
#160=CONTEXT_DEPENDENT_SHAPE_REPRESENTATION(#107,#7900);
#161=CONTEXT_DEPENDENT_SHAPE_REPRESENTATION(#108,#7901);
#162=CONTEXT_DEPENDENT_SHAPE_REPRESENTATION(#109,#7902);
#163=CONTEXT_DEPENDENT_SHAPE_REPRESENTATION(#110,#7903);
#164=CONTEXT_DEPENDENT_SHAPE_REPRESENTATION(#111,#7904);
#165=CONTEXT_DEPENDENT_SHAPE_REPRESENTATION(#112,#7905);
#166=CONTEXT_DEPENDENT_SHAPE_REPRESENTATION(#113,#7906);
#167=CONTEXT_DEPENDENT_SHAPE_REPRESENTATION(#114,#7907);
#168=CONTEXT_DEPENDENT_SHAPE_REPRESENTATION(#115,#7908);
#169=CONTEXT_DEPENDENT_SHAPE_REPRESENTATION(#116,#7909);
#170=NEXT_ASSEMBLY_USAGE_OCCURRENCE('Inner ring:1','Inner ring:1',
'Inner ring:1',#7943,#7944,'Inner ring:1');
#171=NEXT_ASSEMBLY_USAGE_OCCURRENCE('Outer ring:1','Outer ring:1',
'Outer ring:1',#7943,#7945,'Outer ring:1');
#172=NEXT_ASSEMBLY_USAGE_OCCURRENCE('Balls:1','Balls:1','Balls:1',#7943,
#7946,'Balls:1');
#173=NEXT_ASSEMBLY_USAGE_OCCURRENCE('Cage:1','Cage:1','Cage:1',#7943,#7947,
'Cage:1');
#174=NEXT_ASSEMBLY_USAGE_OCCURRENCE('Seals 2RS:1','Seals 2RS:1',
'Seals 2RS:1',#7943,#7948,'Seals 2RS:1');
#175=NEXT_ASSEMBLY_USAGE_OCCURRENCE('Axle:2','Axle:2','Axle:2',#7937,#7938,
'Axle:2');
#176=NEXT_ASSEMBLY_USAGE_OCCURRENCE('Axle Mount A:1','Axle Mount A:1',
'Axle Mount A:1',#7937,#7939,'Axle Mount A:1');
#177=NEXT_ASSEMBLY_USAGE_OCCURRENCE('Slot nut:2','Slot nut:2',
'Slot nut:2',#7937,#7942,'Slot nut:2');
#178=NEXT_ASSEMBLY_USAGE_OCCURRENCE('Slot nut:3','Slot nut:3',
'Slot nut:3',#7937,#7942,'Slot nut:3');
#179=NEXT_ASSEMBLY_USAGE_OCCURRENCE('M5x14 Cap Screw:2',
'M5x14 Cap Screw:2','M5x14 Cap Screw:2',#7937,#7941,'M5x14 Cap Screw:2');
#180=NEXT_ASSEMBLY_USAGE_OCCURRENCE('Axle Mount B:1','Axle Mount B:1',
'Axle Mount B:1',#7937,#7940,'Axle Mount B:1');
#181=NEXT_ASSEMBLY_USAGE_OCCURRENCE('M5x14 Cap Screw:3',
'M5x14 Cap Screw:3','M5x14 Cap Screw:3',#7937,#7941,'M5x14 Cap Screw:3');
#182=NEXT_ASSEMBLY_USAGE_OCCURRENCE('Bearing:3','Bearing:3','Bearing:3',
#7937,#7943,'Bearing:3');
#183=NEXT_ASSEMBLY_USAGE_OCCURRENCE('Cap Screw - M4x16:3',
'Cap Screw - M4x16:3','Cap Screw - M4x16:3',#7937,#7956,
'Cap Screw - M4x16:3');
#184=NEXT_ASSEMBLY_USAGE_OCCURRENCE('Bracket spacer:3',
'Bracket spacer:3','Bracket spacer:3',#7937,#7951,'Bracket spacer:3');
#185=NEXT_ASSEMBLY_USAGE_OCCURRENCE('M5x14 Cap Screw:5',
'M5x14 Cap Screw:5','M5x14 Cap Screw:5',#7937,#7941,'M5x14 Cap Screw:5');
#186=NEXT_ASSEMBLY_USAGE_OCCURRENCE('Slot nut:5','Slot nut:5',
'Slot nut:5',#7937,#7942,'Slot nut:5');
#187=NEXT_ASSEMBLY_USAGE_OCCURRENCE('M5x14 Cap Screw:4',
'M5x14 Cap Screw:4','M5x14 Cap Screw:4',#7937,#7941,'M5x14 Cap Screw:4');
#188=NEXT_ASSEMBLY_USAGE_OCCURRENCE('Slot nut:4','Slot nut:4',
'Slot nut:4',#7937,#7942,'Slot nut:4');
#189=NEXT_ASSEMBLY_USAGE_OCCURRENCE('Spacer:3','Spacer:3','Spacer:3',#7937,
#7950,'Spacer:3');
#190=NEXT_ASSEMBLY_USAGE_OCCURRENCE('End keeper:3','End keeper:3',
'End keeper:3',#7937,#7949,'End keeper:3');
#191=NEXT_ASSEMBLY_USAGE_OCCURRENCE('Bearing:2','Bearing:2','Bearing:2',
#7937,#7943,'Bearing:2');
#192=NEXT_ASSEMBLY_USAGE_OCCURRENCE('End keeper:2','End keeper:2',
'End keeper:2',#7937,#7949,'End keeper:2');
#193=NEXT_ASSEMBLY_USAGE_OCCURRENCE('Spacer:2','Spacer:2','Spacer:2',#7937,
#7950,'Spacer:2');
#194=NEXT_ASSEMBLY_USAGE_OCCURRENCE('Cap Screw - M4x16:2',
'Cap Screw - M4x16:2','Cap Screw - M4x16:2',#7937,#7956,
'Cap Screw - M4x16:2');
#195=NEXT_ASSEMBLY_USAGE_OCCURRENCE('Bracket spacer:2',
'Bracket spacer:2','Bracket spacer:2',#7937,#7951,'Bracket spacer:2');
#196=NEXT_ASSEMBLY_USAGE_OCCURRENCE(
'Slotted Extrusion - 20 x 20 x 300 mm:2',
'Slotted Extrusion - 20 x 20 x 300 mm:2',
'Slotted Extrusion - 20 x 20 x 300 mm:2',#7935,#7936,
'Slotted Extrusion - 20 x 20 x 300 mm:2');
#197=NEXT_ASSEMBLY_USAGE_OCCURRENCE(
'Slotted Extrusion - 20 x 20 x 300 mm:3',
'Slotted Extrusion - 20 x 20 x 300 mm:3',
'Slotted Extrusion - 20 x 20 x 300 mm:3',#7935,#7936,
'Slotted Extrusion - 20 x 20 x 300 mm:3');
#198=NEXT_ASSEMBLY_USAGE_OCCURRENCE('Axle Assembly:1','Axle Assembly:1',
'Axle Assembly:1',#7935,#7937,'Axle Assembly:1');
#199=NEXT_ASSEMBLY_USAGE_OCCURRENCE('Axle Assembly:2','Axle Assembly:2',
'Axle Assembly:2',#7935,#7937,'Axle Assembly:2');
#200=NEXT_ASSEMBLY_USAGE_OCCURRENCE('Axle Assembly:3','Axle Assembly:3',
'Axle Assembly:3',#7935,#7937,'Axle Assembly:3');
#201=NEXT_ASSEMBLY_USAGE_OCCURRENCE('Axle Assembly:4','Axle Assembly:4',
'Axle Assembly:4',#7935,#7937,'Axle Assembly:4');
#202=NEXT_ASSEMBLY_USAGE_OCCURRENCE('Axle Assembly:5','Axle Assembly:5',
'Axle Assembly:5',#7935,#7937,'Axle Assembly:5');
#203=NEXT_ASSEMBLY_USAGE_OCCURRENCE('Axle Assembly:6','Axle Assembly:6',
'Axle Assembly:6',#7935,#7937,'Axle Assembly:6');
#204=NEXT_ASSEMBLY_USAGE_OCCURRENCE('Roller tube:2','Roller tube:2',
'Roller tube:2',#7952,#7953,'Roller tube:2');
#205=NEXT_ASSEMBLY_USAGE_OCCURRENCE('Bearing insert:2',
'Bearing insert:2','Bearing insert:2',#7952,#7954,'Bearing insert:2');
#206=NEXT_ASSEMBLY_USAGE_OCCURRENCE('Bearing insert:3',
'Bearing insert:3','Bearing insert:3',#7952,#7954,'Bearing insert:3');
#207=NEXT_ASSEMBLY_USAGE_OCCURRENCE('Outer race retainer:2',
'Outer race retainer:2','Outer race retainer:2',#7952,#7955,
'Outer race retainer:2');
#208=NEXT_ASSEMBLY_USAGE_OCCURRENCE('Outer race retainer:3',
'Outer race retainer:3','Outer race retainer:3',#7952,#7955,
'Outer race retainer:3');
#209=NEXT_ASSEMBLY_USAGE_OCCURRENCE('Cap Screw - M4x16:4',
'Cap Screw - M4x16:4','Cap Screw - M4x16:4',#7952,#7956,
'Cap Screw - M4x16:4');
#210=NEXT_ASSEMBLY_USAGE_OCCURRENCE('Cap Screw - M4x16:5',
'Cap Screw - M4x16:5','Cap Screw - M4x16:5',#7952,#7956,
'Cap Screw - M4x16:5');
#211=NEXT_ASSEMBLY_USAGE_OCCURRENCE('Cap Screw - M4x16:6',
'Cap Screw - M4x16:6','Cap Screw - M4x16:6',#7952,#7956,
'Cap Screw - M4x16:6');
#212=NEXT_ASSEMBLY_USAGE_OCCURRENCE('Cap Screw - M4x16:7',
'Cap Screw - M4x16:7','Cap Screw - M4x16:7',#7952,#7956,
'Cap Screw - M4x16:7');
#213=NEXT_ASSEMBLY_USAGE_OCCURRENCE('Cap Screw - M4x16:8',
'Cap Screw - M4x16:8','Cap Screw - M4x16:8',#7952,#7956,
'Cap Screw - M4x16:8');
#214=NEXT_ASSEMBLY_USAGE_OCCURRENCE('Cap Screw - M4x16:9',
'Cap Screw - M4x16:9','Cap Screw - M4x16:9',#7952,#7956,
'Cap Screw - M4x16:9');
#215=NEXT_ASSEMBLY_USAGE_OCCURRENCE('Cap Screw - M4x16:10',
'Cap Screw - M4x16:10','Cap Screw - M4x16:10',#7952,#7956,
'Cap Screw - M4x16:10');
#216=NEXT_ASSEMBLY_USAGE_OCCURRENCE('Cap Screw - M4x16:11',
'Cap Screw - M4x16:11','Cap Screw - M4x16:11',#7952,#7956,
'Cap Screw - M4x16:11');
#217=NEXT_ASSEMBLY_USAGE_OCCURRENCE(
'Extrusion frame axles and bearings:1',
'Extrusion frame axles and bearings:1',
'Extrusion frame axles and bearings:1',#7934,#7935,
'Extrusion frame axles and bearings:1');
#218=NEXT_ASSEMBLY_USAGE_OCCURRENCE('Roller Assembly:1',
'Roller Assembly:1','Roller Assembly:1',#7934,#7952,'Roller Assembly:1');
#219=NEXT_ASSEMBLY_USAGE_OCCURRENCE('Roller Assembly:2',
'Roller Assembly:2','Roller Assembly:2',#7934,#7952,'Roller Assembly:2');
#220=NEXT_ASSEMBLY_USAGE_OCCURRENCE('Roller Assembly:3',
'Roller Assembly:3','Roller Assembly:3',#7934,#7952,'Roller Assembly:3');
#221=NEXT_ASSEMBLY_USAGE_OCCURRENCE('Roller Assembly:4',
'Roller Assembly:4','Roller Assembly:4',#7934,#7952,'Roller Assembly:4');
#222=NEXT_ASSEMBLY_USAGE_OCCURRENCE('Roller Assembly:5',
'Roller Assembly:5','Roller Assembly:5',#7934,#7952,'Roller Assembly:5');
#223=B_SPLINE_CURVE_WITH_KNOTS('',3,(#7017,#7018,#7019,#7020,#7021,#7022,
#7023,#7024,#7025,#7026,#7027,#7028,#7029,#7030,#7031,#7032,#7033,#7034,
#7035,#7036,#7037,#7038),.UNSPECIFIED.,.F.,.F.,(4,2,2,2,2,2,2,2,2,2,4),
(0.0473477652366656,0.126350602536658,0.189525903804987,0.252701205073317,
0.313298422430275,0.373895639787233,0.434492857144191,0.495090074501149,
0.558265375769478,0.621440677037807,0.7004435143378),.UNSPECIFIED.);
#224=B_SPLINE_CURVE_WITH_KNOTS('',3,(#7042,#7043,#7044,#7045,#7046,#7047,
#7048,#7049,#7050,#7051,#7052,#7053,#7054,#7055,#7056,#7057,#7058,#7059,
#7060,#7061,#7062,#7063),.UNSPECIFIED.,.F.,.F.,(4,2,2,2,2,2,2,2,2,2,4),
(0.0464897534940957,0.0852567806515119,0.170513561303024,0.246687263103517,
0.308657850341199,0.370628437578881,0.432599024816563,0.494569612054245,
0.570743313854739,0.656000094506251,0.694767121663666),.UNSPECIFIED.);
#225=B_SPLINE_CURVE_WITH_KNOTS('',3,(#7069,#7070,#7071,#7072,#7073,#7074,
#7075,#7076,#7077,#7078,#7079,#7080,#7081,#7082,#7083,#7084,#7085,#7086,
#7087,#7088,#7089,#7090),.UNSPECIFIED.,.F.,.F.,(4,2,2,2,2,2,2,2,2,2,4),
(0.0464897534940957,0.0852567806515118,0.170513561303024,0.246687263103517,
0.308657850341199,0.370628437578881,0.432599024816563,0.494569612054245,
0.570743313854738,0.65600009450625,0.694767121663666),.UNSPECIFIED.);
#226=B_SPLINE_CURVE_WITH_KNOTS('',3,(#7094,#7095,#7096,#7097,#7098,#7099,
#7100,#7101,#7102,#7103,#7104,#7105,#7106,#7107,#7108,#7109,#7110,#7111,
#7112,#7113,#7114,#7115),.UNSPECIFIED.,.F.,.F.,(4,2,2,2,2,2,2,2,2,2,4),
(0.0464897534940957,0.0852567806515119,0.170513561303024,0.246687263103517,
0.308657850341199,0.370628437578881,0.432599024816563,0.494569612054245,
0.570743313854739,0.656000094506251,0.694767121663666),.UNSPECIFIED.);
#227=B_SPLINE_CURVE_WITH_KNOTS('',3,(#7119,#7120,#7121,#7122,#7123,#7124,
#7125,#7126,#7127,#7128,#7129,#7130),.UNSPECIFIED.,.F.,.F.,(4,2,2,2,2,4),
(0.0464897534940957,0.0852567806515119,0.170513561303024,0.246687263103517,
0.308657850341199,0.370628437578881),.UNSPECIFIED.);
#228=B_SPLINE_CURVE_WITH_KNOTS('',3,(#7135,#7136,#7137,#7138,#7139,#7140,
#7141,#7142,#7143,#7144,#7145,#7146),.UNSPECIFIED.,.F.,.F.,(4,2,2,2,2,4),
(0.370628437578881,0.432599024816563,0.494569612054245,0.570743313854738,
0.65600009450625,0.694767121663666),.UNSPECIFIED.);
#229=B_SPLINE_CURVE_WITH_KNOTS('',3,(#7150,#7151,#7152,#7153,#7154,#7155,
#7156,#7157,#7158,#7159,#7160,#7161,#7162,#7163,#7164,#7165,#7166,#7167,
#7168,#7169,#7170,#7171),.UNSPECIFIED.,.F.,.F.,(4,2,2,2,2,2,2,2,2,2,4),
(0.0464897534940957,0.0852567806515121,0.170513561303024,0.246687263103518,
0.308657850341199,0.370628437578881,0.432599024816563,0.494569612054245,
0.570743313854738,0.65600009450625,0.694767121663666),.UNSPECIFIED.);
#230=B_SPLINE_CURVE_WITH_KNOTS('',3,(#7175,#7176,#7177,#7178,#7179,#7180,
#7181,#7182,#7183,#7184,#7185,#7186,#7187,#7188,#7189,#7190,#7191,#7192,
#7193,#7194,#7195,#7196),.UNSPECIFIED.,.F.,.F.,(4,2,2,2,2,2,2,2,2,2,4),
(0.0464897534940957,0.0852567806515119,0.170513561303024,0.246687263103517,
0.308657850341199,0.370628437578881,0.432599024816563,0.494569612054245,
0.570743313854738,0.65600009450625,0.694767121663667),.UNSPECIFIED.);
#231=B_SPLINE_CURVE_WITH_KNOTS('',3,(#7200,#7201,#7202,#7203,#7204,#7205,
#7206,#7207,#7208,#7209,#7210,#7211,#7212,#7213,#7214,#7215,#7216,#7217,
#7218,#7219,#7220,#7221),.UNSPECIFIED.,.F.,.F.,(4,2,2,2,2,2,2,2,2,2,4),
(0.0464897534940957,0.0852567806515119,0.170513561303024,0.246687263103517,
0.308657850341199,0.370628437578881,0.432599024816563,0.494569612054245,
0.570743313854738,0.65600009450625,0.694767121663666),.UNSPECIFIED.);
#232=B_SPLINE_CURVE_WITH_KNOTS('',3,(#7225,#7226,#7227,#7228,#7229,#7230,
#7231,#7232,#7233,#7234,#7235,#7236,#7237,#7238,#7239,#7240,#7241,#7242,
#7243,#7244,#7245,#7246),.UNSPECIFIED.,.F.,.F.,(4,2,2,2,2,2,2,2,2,2,4),
(0.0464897534940957,0.0852567806515119,0.170513561303024,0.246687263103517,
0.308657850341199,0.370628437578881,0.432599024816563,0.494569612054245,
0.570743313854739,0.656000094506251,0.694767121663667),.UNSPECIFIED.);
#233=B_SPLINE_CURVE_WITH_KNOTS('',3,(#7254,#7255,#7256,#7257,#7258,#7259,
#7260,#7261,#7262,#7263,#7264,#7265,#7266,#7267,#7268,#7269,#7270,#7271,
#7272,#7273,#7274,#7275),.UNSPECIFIED.,.F.,.F.,(4,2,2,2,2,2,2,2,2,2,4),
(0.0473477652366656,0.126350602536658,0.189525903804987,0.252701205073316,
0.313298422430274,0.373895639787232,0.434492857144191,0.495090074501149,
0.558265375769478,0.621440677037807,0.7004435143378),.UNSPECIFIED.);
#234=B_SPLINE_CURVE_WITH_KNOTS('',3,(#7283,#7284,#7285,#7286,#7287,#7288,
#7289,#7290,#7291,#7292,#7293,#7294,#7295,#7296,#7297,#7298,#7299,#7300,
#7301,#7302,#7303,#7304),.UNSPECIFIED.,.F.,.F.,(4,2,2,2,2,2,2,2,2,2,4),
(0.0473477652366656,0.126350602536658,0.189525903804987,0.252701205073317,
0.313298422430275,0.373895639787233,0.434492857144191,0.495090074501149,
0.558265375769478,0.621440677037807,0.7004435143378),.UNSPECIFIED.);
#235=B_SPLINE_CURVE_WITH_KNOTS('',3,(#7313,#7314,#7315,#7316,#7317,#7318,
#7319,#7320,#7321,#7322,#7323,#7324),.UNSPECIFIED.,.F.,.F.,(4,2,2,2,2,4),
(0.0473477652366656,0.126350602536658,0.189525903804987,0.252701205073316,
0.313298422430275,0.373895639787233),.UNSPECIFIED.);
#236=B_SPLINE_CURVE_WITH_KNOTS('',3,(#7326,#7327,#7328,#7329,#7330,#7331,
#7332,#7333,#7334,#7335,#7336,#7337),.UNSPECIFIED.,.F.,.F.,(4,2,2,2,2,4),
(0.373895639787233,0.434492857144191,0.495090074501149,0.558265375769478,
0.621440677037807,0.7004435143378),.UNSPECIFIED.);
#237=B_SPLINE_CURVE_WITH_KNOTS('',3,(#7344,#7345,#7346,#7347,#7348,#7349,
#7350,#7351,#7352,#7353,#7354,#7355,#7356,#7357,#7358,#7359,#7360,#7361,
#7362,#7363,#7364,#7365),.UNSPECIFIED.,.F.,.F.,(4,2,2,2,2,2,2,2,2,2,4),
(0.0473477652366656,0.126350602536658,0.189525903804987,0.252701205073316,
0.313298422430275,0.373895639787233,0.434492857144191,0.495090074501149,
0.558265375769478,0.621440677037807,0.7004435143378),.UNSPECIFIED.);
#238=B_SPLINE_CURVE_WITH_KNOTS('',3,(#7373,#7374,#7375,#7376,#7377,#7378,
#7379,#7380,#7381,#7382,#7383,#7384,#7385,#7386,#7387,#7388,#7389,#7390,
#7391,#7392,#7393,#7394),.UNSPECIFIED.,.F.,.F.,(4,2,2,2,2,2,2,2,2,2,4),
(0.0473477652366656,0.126350602536658,0.189525903804987,0.252701205073317,
0.313298422430275,0.373895639787233,0.434492857144191,0.495090074501149,
0.558265375769478,0.621440677037807,0.7004435143378),.UNSPECIFIED.);
#239=B_SPLINE_CURVE_WITH_KNOTS('',3,(#7402,#7403,#7404,#7405,#7406,#7407,
#7408,#7409,#7410,#7411,#7412,#7413,#7414,#7415,#7416,#7417,#7418,#7419,
#7420,#7421,#7422,#7423),.UNSPECIFIED.,.F.,.F.,(4,2,2,2,2,2,2,2,2,2,4),
(0.0473477652366656,0.126350602536658,0.189525903804987,0.252701205073316,
0.313298422430275,0.373895639787233,0.434492857144191,0.495090074501149,
0.558265375769478,0.621440677037807,0.7004435143378),.UNSPECIFIED.);
#240=B_SPLINE_CURVE_WITH_KNOTS('',3,(#7432,#7433,#7434,#7435,#7436,#7437,
#7438,#7439,#7440,#7441,#7442,#7443,#7444,#7445,#7446,#7447,#7448,#7449,
#7450,#7451,#7452,#7453),.UNSPECIFIED.,.F.,.F.,(4,2,2,2,2,2,2,2,2,2,4),
(0.0473477652366656,0.126350602536658,0.189525903804987,0.252701205073317,
0.313298422430275,0.373895639787233,0.434492857144191,0.495090074501149,
0.558265375769478,0.621440677037807,0.7004435143378),.UNSPECIFIED.);
#241=SPHERICAL_SURFACE('',#4660,0.23815);
#242=SPHERICAL_SURFACE('',#4662,0.23815);
#243=SPHERICAL_SURFACE('',#4664,0.23815);
#244=SPHERICAL_SURFACE('',#4666,0.23815);
#245=SPHERICAL_SURFACE('',#4668,0.23815);
#246=SPHERICAL_SURFACE('',#4670,0.23815);
#247=SPHERICAL_SURFACE('',#4672,0.23815);
#248=SPHERICAL_SURFACE('',#4674,0.23815);
#249=SPHERICAL_SURFACE('',#4677,0.247676);
#250=SPHERICAL_SURFACE('',#4693,0.247676);
#251=SPHERICAL_SURFACE('',#4698,0.247676);
#252=SPHERICAL_SURFACE('',#4703,0.247676);
#253=SPHERICAL_SURFACE('',#4708,0.247676);
#254=SPHERICAL_SURFACE('',#4713,0.247676);
#255=SPHERICAL_SURFACE('',#4718,0.247676);
#256=SPHERICAL_SURFACE('',#4726,0.247676);
#257=TOROIDAL_SURFACE('',#4620,1.,0.247676);
#258=TOROIDAL_SURFACE('',#4640,1.,0.247676);
#259=ELLIPSE('',#4608,0.299389011154384,0.2117);
#260=ELLIPSE('',#4612,0.299389011154384,0.2117);
#261=CONICAL_SURFACE('',#4586,0.4,0.785398163397448);
#262=CONICAL_SURFACE('',#4590,0.41,0.785398163397448);
#263=CONICAL_SURFACE('',#4594,0.26,0.463647609000806);
#264=CONICAL_SURFACE('',#4631,0.53,0.785398163397448);
#265=CONICAL_SURFACE('',#4638,0.53,0.785398163397448);
#266=CONICAL_SURFACE('',#4651,1.47,0.785398163397449);
#267=CONICAL_SURFACE('',#4655,1.47,0.785398163397449);
#268=CONICAL_SURFACE('',#4838,0.325,0.785398163397448);
#269=CONICAL_SURFACE('',#4842,0.335,0.785398163397448);
#270=CONICAL_SURFACE('',#4846,0.21,0.463647609000806);
#271=CONICAL_SURFACE('',#4850,0.18,0.785398163397448);
#272=ORIENTED_CLOSED_SHELL('',*,#4203,.F.);
#273=ORIENTED_CLOSED_SHELL('',*,#4226,.F.);
#274=BREP_WITH_VOIDS('Body1',#4204,(#272));
#275=BREP_WITH_VOIDS('Body1',#4225,(#273));
#276=SHAPE_REPRESENTATION_RELATIONSHIP('SRR','None',#7912,#294);
#277=SHAPE_REPRESENTATION_RELATIONSHIP('SRR','None',#7914,#295);
#278=SHAPE_REPRESENTATION_RELATIONSHIP('SRR','None',#7915,#296);
#279=SHAPE_REPRESENTATION_RELATIONSHIP('SRR','None',#7916,#297);
#280=SHAPE_REPRESENTATION_RELATIONSHIP('SRR','None',#7917,#298);
#281=SHAPE_REPRESENTATION_RELATIONSHIP('SRR','None',#7918,#299);
#282=SHAPE_REPRESENTATION_RELATIONSHIP('SRR','None',#7920,#300);
#283=SHAPE_REPRESENTATION_RELATIONSHIP('SRR','None',#7921,#301);
#284=SHAPE_REPRESENTATION_RELATIONSHIP('SRR','None',#7922,#302);
#285=SHAPE_REPRESENTATION_RELATIONSHIP('SRR','None',#7923,#303);
#286=SHAPE_REPRESENTATION_RELATIONSHIP('SRR','None',#7924,#304);
#287=SHAPE_REPRESENTATION_RELATIONSHIP('SRR','None',#7925,#305);
#288=SHAPE_REPRESENTATION_RELATIONSHIP('SRR','None',#7926,#306);
#289=SHAPE_REPRESENTATION_RELATIONSHIP('SRR','None',#7927,#307);
#290=SHAPE_REPRESENTATION_RELATIONSHIP('SRR','None',#7929,#308);
#291=SHAPE_REPRESENTATION_RELATIONSHIP('SRR','None',#7930,#309);
#292=SHAPE_REPRESENTATION_RELATIONSHIP('SRR','None',#7931,#310);
#293=SHAPE_REPRESENTATION_RELATIONSHIP('SRR','None',#7932,#311);
#294=ADVANCED_BREP_SHAPE_REPRESENTATION('',(#338),#7785);
#295=ADVANCED_BREP_SHAPE_REPRESENTATION('',(#339),#7787);
#296=ADVANCED_BREP_SHAPE_REPRESENTATION('',(#340),#7788);
#297=ADVANCED_BREP_SHAPE_REPRESENTATION('',(#341),#7789);
#298=ADVANCED_BREP_SHAPE_REPRESENTATION('',(#274),#7790);
#299=ADVANCED_BREP_SHAPE_REPRESENTATION('',(#342),#7791);
#300=ADVANCED_BREP_SHAPE_REPRESENTATION('',(#343),#7793);
#301=ADVANCED_BREP_SHAPE_REPRESENTATION('',(#344),#7794);
#302=ADVANCED_BREP_SHAPE_REPRESENTATION('',(#345,#346,#347,#348,#349,#350,
#351,#352),#7795);
#303=ADVANCED_BREP_SHAPE_REPRESENTATION('',(#353),#7796);
#304=ADVANCED_BREP_SHAPE_REPRESENTATION('',(#354,#355),#7797);
#305=ADVANCED_BREP_SHAPE_REPRESENTATION('',(#356),#7798);
#306=ADVANCED_BREP_SHAPE_REPRESENTATION('',(#357),#7799);
#307=ADVANCED_BREP_SHAPE_REPRESENTATION('',(#358),#7800);
#308=ADVANCED_BREP_SHAPE_REPRESENTATION('',(#359),#7802);
#309=ADVANCED_BREP_SHAPE_REPRESENTATION('',(#360),#7803);
#310=ADVANCED_BREP_SHAPE_REPRESENTATION('',(#361),#7804);
#311=ADVANCED_BREP_SHAPE_REPRESENTATION('',(#275),#7805);
#312=STYLED_ITEM('',(#8105),#338);
#313=STYLED_ITEM('',(#8091),#339);
#314=STYLED_ITEM('',(#8091),#340);
#315=STYLED_ITEM('',(#8091),#341);
#316=STYLED_ITEM('',(#8098),#274);
#317=STYLED_ITEM('',(#8098),#342);
#318=STYLED_ITEM('',(#8091),#343);
#319=STYLED_ITEM('',(#8091),#344);
#320=STYLED_ITEM('',(#8091),#345);
#321=STYLED_ITEM('',(#8091),#346);
#322=STYLED_ITEM('',(#8091),#347);
#323=STYLED_ITEM('',(#8091),#348);
#324=STYLED_ITEM('',(#8091),#349);
#325=STYLED_ITEM('',(#8091),#350);
#326=STYLED_ITEM('',(#8091),#351);
#327=STYLED_ITEM('',(#8091),#352);
#328=STYLED_ITEM('',(#8091),#353);
#329=STYLED_ITEM('',(#8091),#354);
#330=STYLED_ITEM('',(#8091),#355);
#331=STYLED_ITEM('',(#8105),#356);
#332=STYLED_ITEM('',(#8084),#357);
#333=STYLED_ITEM('',(#8070),#358);
#334=STYLED_ITEM('',(#8077),#359);
#335=STYLED_ITEM('',(#8091),#360);
#336=STYLED_ITEM('',(#8091),#361);
#337=STYLED_ITEM('',(#8098),#275);
#338=MANIFOLD_SOLID_BREP('Body1',#4199);
#339=MANIFOLD_SOLID_BREP('Body1',#4200);
#340=MANIFOLD_SOLID_BREP('Body1',#4201);
#341=MANIFOLD_SOLID_BREP('Body1',#4202);
#342=MANIFOLD_SOLID_BREP('Body1',#4205);
#343=MANIFOLD_SOLID_BREP('Body1',#4206);
#344=MANIFOLD_SOLID_BREP('Body1',#4207);
#345=MANIFOLD_SOLID_BREP('Body1',#4208);
#346=MANIFOLD_SOLID_BREP('Body2',#4209);
#347=MANIFOLD_SOLID_BREP('Body3',#4210);
#348=MANIFOLD_SOLID_BREP('Body4',#4211);
#349=MANIFOLD_SOLID_BREP('Body5',#4212);
#350=MANIFOLD_SOLID_BREP('Body6',#4213);
#351=MANIFOLD_SOLID_BREP('Body7',#4214);
#352=MANIFOLD_SOLID_BREP('Body8',#4215);
#353=MANIFOLD_SOLID_BREP('Continuous crown cage',#4216);
#354=MANIFOLD_SOLID_BREP('Body1',#4217);
#355=MANIFOLD_SOLID_BREP('Body2',#4218);
#356=MANIFOLD_SOLID_BREP('Body1',#4219);
#357=MANIFOLD_SOLID_BREP('Body1',#4220);
#358=MANIFOLD_SOLID_BREP('Body1',#4221);
#359=MANIFOLD_SOLID_BREP('Body1',#4222);
#360=MANIFOLD_SOLID_BREP('Body1',#4223);
#361=MANIFOLD_SOLID_BREP('Body1',#4224);
#362=FACE_BOUND('',#930,.T.);
#363=FACE_BOUND('',#932,.T.);
#364=FACE_BOUND('',#938,.T.);
#365=FACE_BOUND('',#940,.T.);
#366=FACE_BOUND('',#945,.T.);
#367=FACE_BOUND('',#947,.T.);
#368=FACE_BOUND('',#951,.T.);
#369=FACE_BOUND('',#955,.T.);
#370=FACE_BOUND('',#957,.T.);
#371=FACE_BOUND('',#969,.T.);
#372=FACE_BOUND('',#973,.T.);
#373=FACE_BOUND('',#974,.T.);
#374=FACE_BOUND('',#978,.T.);
#375=FACE_BOUND('',#982,.T.);
#376=FACE_BOUND('',#984,.T.);
#377=FACE_BOUND('',#996,.T.);
#378=FACE_BOUND('',#1000,.T.);
#379=FACE_BOUND('',#1001,.T.);
#380=FACE_BOUND('',#1016,.T.);
#381=FACE_BOUND('',#1022,.T.);
#382=FACE_BOUND('',#1039,.T.);
#383=FACE_BOUND('',#1042,.T.);
#384=FACE_BOUND('',#1047,.T.);
#385=FACE_BOUND('',#1052,.T.);
#386=FACE_BOUND('',#1080,.T.);
#387=FACE_BOUND('',#1083,.T.);
#388=FACE_BOUND('',#1086,.T.);
#389=FACE_BOUND('',#1089,.T.);
#390=FACE_BOUND('',#1092,.T.);
#391=FACE_BOUND('',#1097,.T.);
#392=FACE_BOUND('',#1099,.T.);
#393=FACE_BOUND('',#1103,.T.);
#394=FACE_BOUND('',#1105,.T.);
#395=FACE_BOUND('',#1109,.T.);
#396=FACE_BOUND('',#1111,.T.);
#397=FACE_BOUND('',#1115,.T.);
#398=FACE_BOUND('',#1117,.T.);
#399=FACE_BOUND('',#1124,.T.);
#400=FACE_BOUND('',#1128,.T.);
#401=FACE_BOUND('',#1129,.T.);
#402=FACE_BOUND('',#1130,.T.);
#403=FACE_BOUND('',#1131,.T.);
#404=FACE_BOUND('',#1132,.T.);
#405=FACE_BOUND('',#1134,.T.);
#406=FACE_BOUND('',#1135,.T.);
#407=FACE_BOUND('',#1136,.T.);
#408=FACE_BOUND('',#1137,.T.);
#409=FACE_BOUND('',#1138,.T.);
#410=FACE_BOUND('',#1146,.T.);
#411=FACE_BOUND('',#1147,.T.);
#412=FACE_BOUND('',#1148,.T.);
#413=FACE_BOUND('',#1149,.T.);
#414=FACE_BOUND('',#1150,.T.);
#415=FACE_BOUND('',#1152,.T.);
#416=FACE_BOUND('',#1153,.T.);
#417=FACE_BOUND('',#1154,.T.);
#418=FACE_BOUND('',#1155,.T.);
#419=FACE_BOUND('',#1156,.T.);
#420=FACE_BOUND('',#1162,.T.);
#421=CIRCLE('',#4466,0.21);
#422=CIRCLE('',#4467,0.21);
#423=CIRCLE('',#4481,0.165);
#424=CIRCLE('',#4482,0.165);
#425=CIRCLE('',#4485,0.165);
#426=CIRCLE('',#4486,0.165);
#427=CIRCLE('',#4489,0.6);
#428=CIRCLE('',#4490,0.5);
#429=CIRCLE('',#4492,0.6);
#430=CIRCLE('',#4493,0.5);
#431=CIRCLE('',#4496,0.5);
#432=CIRCLE('',#4498,0.5);
#433=CIRCLE('',#4503,0.5);
#434=CIRCLE('',#4504,0.5);
#435=CIRCLE('',#4506,0.5);
#436=CIRCLE('',#4507,0.5);
#437=CIRCLE('',#4509,0.275);
#438=CIRCLE('',#4511,0.5);
#439=CIRCLE('',#4512,0.5);
#440=CIRCLE('',#4514,0.5);
#441=CIRCLE('',#4515,0.5);
#442=CIRCLE('',#4517,0.275);
#443=CIRCLE('',#4519,0.505);
#444=CIRCLE('',#4524,0.275);
#445=CIRCLE('',#4526,0.275);
#446=CIRCLE('',#4528,0.505);
#447=CIRCLE('',#4539,0.5);
#448=CIRCLE('',#4540,0.5);
#449=CIRCLE('',#4542,0.5);
#450=CIRCLE('',#4543,0.5);
#451=CIRCLE('',#4545,0.275);
#452=CIRCLE('',#4547,0.5);
#453=CIRCLE('',#4548,0.5);
#454=CIRCLE('',#4550,0.5);
#455=CIRCLE('',#4551,0.5);
#456=CIRCLE('',#4553,0.275);
#457=CIRCLE('',#4555,0.505);
#458=CIRCLE('',#4560,0.275);
#459=CIRCLE('',#4562,0.275);
#460=CIRCLE('',#4564,0.505);
#461=CIRCLE('',#4583,0.24505);
#462=CIRCLE('',#4585,0.375);
#463=CIRCLE('',#4587,0.425);
#464=CIRCLE('',#4589,0.425);
#465=CIRCLE('',#4591,0.395);
#466=CIRCLE('',#4593,0.27);
#467=CIRCLE('',#4595,0.24505);
#468=CIRCLE('',#4601,0.2117);
#469=CIRCLE('',#4610,0.2117);
#470=CIRCLE('',#4611,0.2117);
#471=CIRCLE('',#4613,0.2117);
#472=CIRCLE('',#4621,0.976185);
#473=CIRCLE('',#4622,0.976185);
#474=CIRCLE('',#4623,0.247676);
#475=CIRCLE('',#4624,0.976185);
#476=CIRCLE('',#4625,0.976185);
#477=CIRCLE('',#4627,0.976185);
#478=CIRCLE('',#4629,0.5);
#479=CIRCLE('',#4630,0.5);
#480=CIRCLE('',#4632,0.56);
#481=CIRCLE('',#4635,0.976185);
#482=CIRCLE('',#4637,0.56);
#483=CIRCLE('',#4641,1.023815);
#484=CIRCLE('',#4642,1.023815);
#485=CIRCLE('',#4643,0.247676);
#486=CIRCLE('',#4644,1.023815);
#487=CIRCLE('',#4645,1.023815);
#488=CIRCLE('',#4647,1.023815);
#489=CIRCLE('',#4649,1.44);
#490=CIRCLE('',#4650,1.023815);
#491=CIRCLE('',#4652,1.5);
#492=CIRCLE('',#4654,1.5);
#493=CIRCLE('',#4656,1.44);
#494=CIRCLE('',#4661,0.23815);
#495=CIRCLE('',#4663,0.23815);
#496=CIRCLE('',#4665,0.23815);
#497=CIRCLE('',#4667,0.23815);
#498=CIRCLE('',#4669,0.23815);
#499=CIRCLE('',#4671,0.23815);
#500=CIRCLE('',#4673,0.23815);
#501=CIRCLE('',#4675,0.23815);
#502=CIRCLE('',#4678,0.243053047864041);
#503=CIRCLE('',#4679,0.243053047864041);
#504=CIRCLE('',#4681,1.019052);
#505=CIRCLE('',#4682,1.019052);
#506=CIRCLE('',#4683,1.019052);
#507=CIRCLE('',#4684,1.019052);
#508=CIRCLE('',#4685,1.019052);
#509=CIRCLE('',#4686,1.019052);
#510=CIRCLE('',#4687,1.019052);
#511=CIRCLE('',#4688,1.019052);
#512=CIRCLE('',#4689,1.019052);
#513=CIRCLE('',#4691,0.980948);
#514=CIRCLE('',#4692,0.243053047864041);
#515=CIRCLE('',#4694,0.243053047864041);
#516=CIRCLE('',#4696,0.980948);
#517=CIRCLE('',#4697,0.243053047864041);
#518=CIRCLE('',#4699,0.243053047864041);
#519=CIRCLE('',#4701,0.980948);
#520=CIRCLE('',#4702,0.243053047864041);
#521=CIRCLE('',#4704,0.243053047864041);
#522=CIRCLE('',#4706,0.980948);
#523=CIRCLE('',#4707,0.243053047864041);
#524=CIRCLE('',#4709,0.243053047864041);
#525=CIRCLE('',#4711,0.980948);
#526=CIRCLE('',#4712,0.243053047864041);
#527=CIRCLE('',#4714,0.243053047864041);
#528=CIRCLE('',#4716,0.980948);
#529=CIRCLE('',#4717,0.243053047864041);
#530=CIRCLE('',#4719,0.243053047864041);
#531=CIRCLE('',#4721,0.980948);
#532=CIRCLE('',#4722,0.980948);
#533=CIRCLE('',#4723,0.980948);
#534=CIRCLE('',#4725,0.243053047864041);
#535=CIRCLE('',#4727,0.243053047864041);
#536=CIRCLE('',#4732,1.013815);
#537=CIRCLE('',#4733,0.991185);
#538=CIRCLE('',#4735,1.013815);
#539=CIRCLE('',#4737,0.991185);
#540=CIRCLE('',#4740,1.013815);
#541=CIRCLE('',#4741,0.991185);
#542=CIRCLE('',#4743,1.013815);
#543=CIRCLE('',#4745,0.991185);
#544=CIRCLE('',#4754,0.225);
#545=CIRCLE('',#4755,0.225);
#546=CIRCLE('',#4757,1.1);
#547=CIRCLE('',#4758,1.1);
#548=CIRCLE('',#4763,0.505);
#549=CIRCLE('',#4764,0.505);
#550=CIRCLE('',#4766,0.8);
#551=CIRCLE('',#4767,0.8);
#552=CIRCLE('',#4772,0.605);
#553=CIRCLE('',#4773,0.605);
#554=CIRCLE('',#4775,1.);
#555=CIRCLE('',#4776,1.);
#556=CIRCLE('',#4782,2.2);
#557=CIRCLE('',#4783,2.2);
#558=CIRCLE('',#4785,2.5);
#559=CIRCLE('',#4786,2.5);
#560=CIRCLE('',#4791,0.165);
#561=CIRCLE('',#4792,0.165);
#562=CIRCLE('',#4794,0.165);
#563=CIRCLE('',#4795,0.165);
#564=CIRCLE('',#4797,0.165);
#565=CIRCLE('',#4798,0.165);
#566=CIRCLE('',#4800,0.165);
#567=CIRCLE('',#4801,0.165);
#568=CIRCLE('',#4803,1.2);
#569=CIRCLE('',#4804,1.2);
#570=CIRCLE('',#4806,1.5);
#571=CIRCLE('',#4808,1.5);
#572=CIRCLE('',#4810,2.2);
#573=CIRCLE('',#4811,2.2);
#574=CIRCLE('',#4816,0.225);
#575=CIRCLE('',#4817,0.225);
#576=CIRCLE('',#4819,0.225);
#577=CIRCLE('',#4820,0.225);
#578=CIRCLE('',#4822,0.225);
#579=CIRCLE('',#4823,0.225);
#580=CIRCLE('',#4825,0.225);
#581=CIRCLE('',#4826,0.225);
#582=CIRCLE('',#4828,1.2);
#583=CIRCLE('',#4829,1.2);
#584=CIRCLE('',#4831,2.5);
#585=CIRCLE('',#4832,2.5);
#586=CIRCLE('',#4837,0.3);
#587=CIRCLE('',#4839,0.35);
#588=CIRCLE('',#4841,0.35);
#589=CIRCLE('',#4843,0.32);
#590=CIRCLE('',#4845,0.22);
#591=CIRCLE('',#4847,0.1954);
#592=CIRCLE('',#4849,0.1954);
#593=CIRCLE('',#4851,0.16);
#594=CYLINDRICAL_SURFACE('',#4465,0.21);
#595=CYLINDRICAL_SURFACE('',#4480,0.165);
#596=CYLINDRICAL_SURFACE('',#4484,0.165);
#597=CYLINDRICAL_SURFACE('',#4494,0.6);
#598=CYLINDRICAL_SURFACE('',#4495,0.5);
#599=CYLINDRICAL_SURFACE('',#4497,0.5);
#600=CYLINDRICAL_SURFACE('',#4502,0.5);
#601=CYLINDRICAL_SURFACE('',#4505,0.5);
#602=CYLINDRICAL_SURFACE('',#4510,0.5);
#603=CYLINDRICAL_SURFACE('',#4513,0.5);
#604=CYLINDRICAL_SURFACE('',#4523,0.275);
#605=CYLINDRICAL_SURFACE('',#4525,0.275);
#606=CYLINDRICAL_SURFACE('',#4527,0.505);
#607=CYLINDRICAL_SURFACE('',#4538,0.5);
#608=CYLINDRICAL_SURFACE('',#4541,0.5);
#609=CYLINDRICAL_SURFACE('',#4546,0.5);
#610=CYLINDRICAL_SURFACE('',#4549,0.5);
#611=CYLINDRICAL_SURFACE('',#4559,0.275);
#612=CYLINDRICAL_SURFACE('',#4561,0.275);
#613=CYLINDRICAL_SURFACE('',#4563,0.505);
#614=CYLINDRICAL_SURFACE('',#4588,0.425);
#615=CYLINDRICAL_SURFACE('',#4596,0.24505);
#616=CYLINDRICAL_SURFACE('',#4609,0.2117);
#617=CYLINDRICAL_SURFACE('',#4626,0.976185);
#618=CYLINDRICAL_SURFACE('',#4628,0.5);
#619=CYLINDRICAL_SURFACE('',#4634,0.976185);
#620=CYLINDRICAL_SURFACE('',#4646,1.023815);
#621=CYLINDRICAL_SURFACE('',#4653,1.5);
#622=CYLINDRICAL_SURFACE('',#4658,1.023815);
#623=CYLINDRICAL_SURFACE('',#4680,1.019052);
#624=CYLINDRICAL_SURFACE('',#4720,0.980948);
#625=CYLINDRICAL_SURFACE('',#4734,1.013815);
#626=CYLINDRICAL_SURFACE('',#4738,0.991185);
#627=CYLINDRICAL_SURFACE('',#4742,1.013815);
#628=CYLINDRICAL_SURFACE('',#4746,0.991185);
#629=CYLINDRICAL_SURFACE('',#4753,0.225);
#630=CYLINDRICAL_SURFACE('',#4756,1.1);
#631=CYLINDRICAL_SURFACE('',#4762,0.505);
#632=CYLINDRICAL_SURFACE('',#4765,0.8);
#633=CYLINDRICAL_SURFACE('',#4771,0.605);
#634=CYLINDRICAL_SURFACE('',#4774,1.);
#635=CYLINDRICAL_SURFACE('',#4781,2.2);
#636=CYLINDRICAL_SURFACE('',#4784,2.5);
#637=CYLINDRICAL_SURFACE('',#4790,0.165);
#638=CYLINDRICAL_SURFACE('',#4793,0.165);
#639=CYLINDRICAL_SURFACE('',#4796,0.165);
#640=CYLINDRICAL_SURFACE('',#4799,0.165);
#641=CYLINDRICAL_SURFACE('',#4802,1.2);
#642=CYLINDRICAL_SURFACE('',#4807,1.5);
#643=CYLINDRICAL_SURFACE('',#4809,2.2);
#644=CYLINDRICAL_SURFACE('',#4815,0.225);
#645=CYLINDRICAL_SURFACE('',#4818,0.225);
#646=CYLINDRICAL_SURFACE('',#4821,0.225);
#647=CYLINDRICAL_SURFACE('',#4824,0.225);
#648=CYLINDRICAL_SURFACE('',#4827,1.2);
#649=CYLINDRICAL_SURFACE('',#4830,2.5);
#650=CYLINDRICAL_SURFACE('',#4840,0.35);
#651=CYLINDRICAL_SURFACE('',#4848,0.1954);
#652=FACE_OUTER_BOUND('',#884,.T.);
#653=FACE_OUTER_BOUND('',#885,.T.);
#654=FACE_OUTER_BOUND('',#886,.T.);
#655=FACE_OUTER_BOUND('',#887,.T.);
#656=FACE_OUTER_BOUND('',#888,.T.);
#657=FACE_OUTER_BOUND('',#889,.T.);
#658=FACE_OUTER_BOUND('',#890,.T.);
#659=FACE_OUTER_BOUND('',#891,.T.);
#660=FACE_OUTER_BOUND('',#892,.T.);
#661=FACE_OUTER_BOUND('',#893,.T.);
#662=FACE_OUTER_BOUND('',#894,.T.);
#663=FACE_OUTER_BOUND('',#895,.T.);
#664=FACE_OUTER_BOUND('',#896,.T.);
#665=FACE_OUTER_BOUND('',#897,.T.);
#666=FACE_OUTER_BOUND('',#898,.T.);
#667=FACE_OUTER_BOUND('',#899,.T.);
#668=FACE_OUTER_BOUND('',#900,.T.);
#669=FACE_OUTER_BOUND('',#901,.T.);
#670=FACE_OUTER_BOUND('',#902,.T.);
#671=FACE_OUTER_BOUND('',#903,.T.);
#672=FACE_OUTER_BOUND('',#904,.T.);
#673=FACE_OUTER_BOUND('',#905,.T.);
#674=FACE_OUTER_BOUND('',#906,.T.);
#675=FACE_OUTER_BOUND('',#907,.T.);
#676=FACE_OUTER_BOUND('',#908,.T.);
#677=FACE_OUTER_BOUND('',#909,.T.);
#678=FACE_OUTER_BOUND('',#910,.T.);
#679=FACE_OUTER_BOUND('',#911,.T.);
#680=FACE_OUTER_BOUND('',#912,.T.);
#681=FACE_OUTER_BOUND('',#913,.T.);
#682=FACE_OUTER_BOUND('',#914,.T.);
#683=FACE_OUTER_BOUND('',#915,.T.);
#684=FACE_OUTER_BOUND('',#916,.T.);
#685=FACE_OUTER_BOUND('',#917,.T.);
#686=FACE_OUTER_BOUND('',#918,.T.);
#687=FACE_OUTER_BOUND('',#919,.T.);
#688=FACE_OUTER_BOUND('',#920,.T.);
#689=FACE_OUTER_BOUND('',#921,.T.);
#690=FACE_OUTER_BOUND('',#922,.T.);
#691=FACE_OUTER_BOUND('',#923,.T.);
#692=FACE_OUTER_BOUND('',#924,.T.);
#693=FACE_OUTER_BOUND('',#925,.T.);
#694=FACE_OUTER_BOUND('',#926,.T.);
#695=FACE_OUTER_BOUND('',#927,.T.);
#696=FACE_OUTER_BOUND('',#928,.T.);
#697=FACE_OUTER_BOUND('',#929,.T.);
#698=FACE_OUTER_BOUND('',#931,.T.);
#699=FACE_OUTER_BOUND('',#933,.T.);
#700=FACE_OUTER_BOUND('',#934,.T.);
#701=FACE_OUTER_BOUND('',#935,.T.);
#702=FACE_OUTER_BOUND('',#936,.T.);
#703=FACE_OUTER_BOUND('',#937,.T.);
#704=FACE_OUTER_BOUND('',#939,.T.);
#705=FACE_OUTER_BOUND('',#941,.T.);
#706=FACE_OUTER_BOUND('',#942,.T.);
#707=FACE_OUTER_BOUND('',#943,.T.);
#708=FACE_OUTER_BOUND('',#944,.T.);
#709=FACE_OUTER_BOUND('',#946,.T.);
#710=FACE_OUTER_BOUND('',#948,.T.);
#711=FACE_OUTER_BOUND('',#949,.T.);
#712=FACE_OUTER_BOUND('',#950,.T.);
#713=FACE_OUTER_BOUND('',#952,.T.);
#714=FACE_OUTER_BOUND('',#953,.T.);
#715=FACE_OUTER_BOUND('',#954,.T.);
#716=FACE_OUTER_BOUND('',#956,.T.);
#717=FACE_OUTER_BOUND('',#958,.T.);
#718=FACE_OUTER_BOUND('',#959,.T.);
#719=FACE_OUTER_BOUND('',#960,.T.);
#720=FACE_OUTER_BOUND('',#961,.T.);
#721=FACE_OUTER_BOUND('',#962,.T.);
#722=FACE_OUTER_BOUND('',#963,.T.);
#723=FACE_OUTER_BOUND('',#964,.T.);
#724=FACE_OUTER_BOUND('',#965,.T.);
#725=FACE_OUTER_BOUND('',#966,.T.);
#726=FACE_OUTER_BOUND('',#967,.T.);
#727=FACE_OUTER_BOUND('',#968,.T.);
#728=FACE_OUTER_BOUND('',#970,.T.);
#729=FACE_OUTER_BOUND('',#971,.T.);
#730=FACE_OUTER_BOUND('',#972,.T.);
#731=FACE_OUTER_BOUND('',#975,.T.);
#732=FACE_OUTER_BOUND('',#976,.T.);
#733=FACE_OUTER_BOUND('',#977,.T.);
#734=FACE_OUTER_BOUND('',#979,.T.);
#735=FACE_OUTER_BOUND('',#980,.T.);
#736=FACE_OUTER_BOUND('',#981,.T.);
#737=FACE_OUTER_BOUND('',#983,.T.);
#738=FACE_OUTER_BOUND('',#985,.T.);
#739=FACE_OUTER_BOUND('',#986,.T.);
#740=FACE_OUTER_BOUND('',#987,.T.);
#741=FACE_OUTER_BOUND('',#988,.T.);
#742=FACE_OUTER_BOUND('',#989,.T.);
#743=FACE_OUTER_BOUND('',#990,.T.);
#744=FACE_OUTER_BOUND('',#991,.T.);
#745=FACE_OUTER_BOUND('',#992,.T.);
#746=FACE_OUTER_BOUND('',#993,.T.);
#747=FACE_OUTER_BOUND('',#994,.T.);
#748=FACE_OUTER_BOUND('',#995,.T.);
#749=FACE_OUTER_BOUND('',#997,.T.);
#750=FACE_OUTER_BOUND('',#998,.T.);
#751=FACE_OUTER_BOUND('',#999,.T.);
#752=FACE_OUTER_BOUND('',#1002,.T.);
#753=FACE_OUTER_BOUND('',#1003,.T.);
#754=FACE_OUTER_BOUND('',#1004,.T.);
#755=FACE_OUTER_BOUND('',#1005,.T.);
#756=FACE_OUTER_BOUND('',#1006,.T.);
#757=FACE_OUTER_BOUND('',#1007,.T.);
#758=FACE_OUTER_BOUND('',#1008,.T.);
#759=FACE_OUTER_BOUND('',#1009,.T.);
#760=FACE_OUTER_BOUND('',#1010,.T.);
#761=FACE_OUTER_BOUND('',#1011,.T.);
#762=FACE_OUTER_BOUND('',#1012,.T.);
#763=FACE_OUTER_BOUND('',#1013,.T.);
#764=FACE_OUTER_BOUND('',#1014,.T.);
#765=FACE_OUTER_BOUND('',#1015,.T.);
#766=FACE_OUTER_BOUND('',#1017,.T.);
#767=FACE_OUTER_BOUND('',#1018,.T.);
#768=FACE_OUTER_BOUND('',#1019,.T.);
#769=FACE_OUTER_BOUND('',#1020,.T.);
#770=FACE_OUTER_BOUND('',#1021,.T.);
#771=FACE_OUTER_BOUND('',#1023,.T.);
#772=FACE_OUTER_BOUND('',#1024,.T.);
#773=FACE_OUTER_BOUND('',#1025,.T.);
#774=FACE_OUTER_BOUND('',#1026,.T.);
#775=FACE_OUTER_BOUND('',#1027,.T.);
#776=FACE_OUTER_BOUND('',#1028,.T.);
#777=FACE_OUTER_BOUND('',#1029,.T.);
#778=FACE_OUTER_BOUND('',#1030,.T.);
#779=FACE_OUTER_BOUND('',#1031,.T.);
#780=FACE_OUTER_BOUND('',#1032,.T.);
#781=FACE_OUTER_BOUND('',#1033,.T.);
#782=FACE_OUTER_BOUND('',#1034,.T.);
#783=FACE_OUTER_BOUND('',#1035,.T.);
#784=FACE_OUTER_BOUND('',#1036,.T.);
#785=FACE_OUTER_BOUND('',#1037,.T.);
#786=FACE_OUTER_BOUND('',#1038,.T.);
#787=FACE_OUTER_BOUND('',#1040,.T.);
#788=FACE_OUTER_BOUND('',#1041,.T.);
#789=FACE_OUTER_BOUND('',#1043,.T.);
#790=FACE_OUTER_BOUND('',#1044,.T.);
#791=FACE_OUTER_BOUND('',#1045,.T.);
#792=FACE_OUTER_BOUND('',#1046,.T.);
#793=FACE_OUTER_BOUND('',#1048,.T.);
#794=FACE_OUTER_BOUND('',#1049,.T.);
#795=FACE_OUTER_BOUND('',#1050,.T.);
#796=FACE_OUTER_BOUND('',#1051,.T.);
#797=FACE_OUTER_BOUND('',#1053,.T.);
#798=FACE_OUTER_BOUND('',#1054,.T.);
#799=FACE_OUTER_BOUND('',#1055,.T.);
#800=FACE_OUTER_BOUND('',#1056,.T.);
#801=FACE_OUTER_BOUND('',#1057,.T.);
#802=FACE_OUTER_BOUND('',#1058,.T.);
#803=FACE_OUTER_BOUND('',#1059,.T.);
#804=FACE_OUTER_BOUND('',#1060,.T.);
#805=FACE_OUTER_BOUND('',#1061,.T.);
#806=FACE_OUTER_BOUND('',#1062,.T.);
#807=FACE_OUTER_BOUND('',#1063,.T.);
#808=FACE_OUTER_BOUND('',#1064,.T.);
#809=FACE_OUTER_BOUND('',#1065,.T.);
#810=FACE_OUTER_BOUND('',#1066,.T.);
#811=FACE_OUTER_BOUND('',#1067,.T.);
#812=FACE_OUTER_BOUND('',#1068,.T.);
#813=FACE_OUTER_BOUND('',#1069,.T.);
#814=FACE_OUTER_BOUND('',#1070,.T.);
#815=FACE_OUTER_BOUND('',#1071,.T.);
#816=FACE_OUTER_BOUND('',#1072,.T.);
#817=FACE_OUTER_BOUND('',#1073,.T.);
#818=FACE_OUTER_BOUND('',#1074,.T.);
#819=FACE_OUTER_BOUND('',#1075,.T.);
#820=FACE_OUTER_BOUND('',#1076,.T.);
#821=FACE_OUTER_BOUND('',#1077,.T.);
#822=FACE_OUTER_BOUND('',#1078,.T.);
#823=FACE_OUTER_BOUND('',#1079,.T.);
#824=FACE_OUTER_BOUND('',#1081,.T.);
#825=FACE_OUTER_BOUND('',#1082,.T.);
#826=FACE_OUTER_BOUND('',#1084,.T.);
#827=FACE_OUTER_BOUND('',#1085,.T.);
#828=FACE_OUTER_BOUND('',#1087,.T.);
#829=FACE_OUTER_BOUND('',#1088,.T.);
#830=FACE_OUTER_BOUND('',#1090,.T.);
#831=FACE_OUTER_BOUND('',#1091,.T.);
#832=FACE_OUTER_BOUND('',#1093,.T.);
#833=FACE_OUTER_BOUND('',#1094,.T.);
#834=FACE_OUTER_BOUND('',#1095,.T.);
#835=FACE_OUTER_BOUND('',#1096,.T.);
#836=FACE_OUTER_BOUND('',#1098,.T.);
#837=FACE_OUTER_BOUND('',#1100,.T.);
#838=FACE_OUTER_BOUND('',#1101,.T.);
#839=FACE_OUTER_BOUND('',#1102,.T.);
#840=FACE_OUTER_BOUND('',#1104,.T.);
#841=FACE_OUTER_BOUND('',#1106,.T.);
#842=FACE_OUTER_BOUND('',#1107,.T.);
#843=FACE_OUTER_BOUND('',#1108,.T.);
#844=FACE_OUTER_BOUND('',#1110,.T.);
#845=FACE_OUTER_BOUND('',#1112,.T.);
#846=FACE_OUTER_BOUND('',#1113,.T.);
#847=FACE_OUTER_BOUND('',#1114,.T.);
#848=FACE_OUTER_BOUND('',#1116,.T.);
#849=FACE_OUTER_BOUND('',#1118,.T.);
#850=FACE_OUTER_BOUND('',#1119,.T.);
#851=FACE_OUTER_BOUND('',#1120,.T.);
#852=FACE_OUTER_BOUND('',#1121,.T.);
#853=FACE_OUTER_BOUND('',#1122,.T.);
#854=FACE_OUTER_BOUND('',#1123,.T.);
#855=FACE_OUTER_BOUND('',#1125,.T.);
#856=FACE_OUTER_BOUND('',#1126,.T.);
#857=FACE_OUTER_BOUND('',#1127,.T.);
#858=FACE_OUTER_BOUND('',#1133,.T.);
#859=FACE_OUTER_BOUND('',#1139,.T.);
#860=FACE_OUTER_BOUND('',#1140,.T.);
#861=FACE_OUTER_BOUND('',#1141,.T.);
#862=FACE_OUTER_BOUND('',#1142,.T.);
#863=FACE_OUTER_BOUND('',#1143,.T.);
#864=FACE_OUTER_BOUND('',#1144,.T.);
#865=FACE_OUTER_BOUND('',#1145,.T.);
#866=FACE_OUTER_BOUND('',#1151,.T.);
#867=FACE_OUTER_BOUND('',#1157,.T.);
#868=FACE_OUTER_BOUND('',#1158,.T.);
#869=FACE_OUTER_BOUND('',#1159,.T.);
#870=FACE_OUTER_BOUND('',#1160,.T.);
#871=FACE_OUTER_BOUND('',#1161,.T.);
#872=FACE_OUTER_BOUND('',#1163,.T.);
#873=FACE_OUTER_BOUND('',#1164,.T.);
#874=FACE_OUTER_BOUND('',#1165,.T.);
#875=FACE_OUTER_BOUND('',#1166,.T.);
#876=FACE_OUTER_BOUND('',#1167,.T.);
#877=FACE_OUTER_BOUND('',#1168,.T.);
#878=FACE_OUTER_BOUND('',#1169,.T.);
#879=FACE_OUTER_BOUND('',#1170,.T.);
#880=FACE_OUTER_BOUND('',#1171,.T.);
#881=FACE_OUTER_BOUND('',#1172,.T.);
#882=FACE_OUTER_BOUND('',#1173,.T.);
#883=FACE_OUTER_BOUND('',#1174,.T.);
#884=EDGE_LOOP('',(#2754,#2755,#2756,#2757));
#885=EDGE_LOOP('',(#2758,#2759,#2760,#2761));
#886=EDGE_LOOP('',(#2762,#2763,#2764,#2765));
#887=EDGE_LOOP('',(#2766,#2767,#2768,#2769));
#888=EDGE_LOOP('',(#2770,#2771,#2772,#2773));
#889=EDGE_LOOP('',(#2774,#2775,#2776,#2777));
#890=EDGE_LOOP('',(#2778,#2779,#2780,#2781));
#891=EDGE_LOOP('',(#2782,#2783,#2784,#2785));
#892=EDGE_LOOP('',(#2786,#2787,#2788,#2789));
#893=EDGE_LOOP('',(#2790,#2791,#2792,#2793));
#894=EDGE_LOOP('',(#2794,#2795,#2796,#2797));
#895=EDGE_LOOP('',(#2798,#2799,#2800,#2801));
#896=EDGE_LOOP('',(#2802,#2803,#2804,#2805));
#897=EDGE_LOOP('',(#2806,#2807,#2808,#2809));
#898=EDGE_LOOP('',(#2810,#2811,#2812,#2813));
#899=EDGE_LOOP('',(#2814,#2815,#2816,#2817));
#900=EDGE_LOOP('',(#2818,#2819,#2820,#2821));
#901=EDGE_LOOP('',(#2822,#2823,#2824,#2825));
#902=EDGE_LOOP('',(#2826,#2827,#2828,#2829));
#903=EDGE_LOOP('',(#2830,#2831,#2832,#2833));
#904=EDGE_LOOP('',(#2834,#2835,#2836,#2837));
#905=EDGE_LOOP('',(#2838,#2839,#2840,#2841));
#906=EDGE_LOOP('',(#2842,#2843,#2844,#2845));
#907=EDGE_LOOP('',(#2846,#2847,#2848,#2849));
#908=EDGE_LOOP('',(#2850,#2851,#2852,#2853));
#909=EDGE_LOOP('',(#2854,#2855,#2856,#2857));
#910=EDGE_LOOP('',(#2858,#2859,#2860,#2861));
#911=EDGE_LOOP('',(#2862,#2863,#2864,#2865));
#912=EDGE_LOOP('',(#2866,#2867,#2868,#2869));
#913=EDGE_LOOP('',(#2870,#2871,#2872,#2873));
#914=EDGE_LOOP('',(#2874,#2875,#2876,#2877));
#915=EDGE_LOOP('',(#2878,#2879,#2880,#2881));
#916=EDGE_LOOP('',(#2882,#2883,#2884,#2885));
#917=EDGE_LOOP('',(#2886,#2887,#2888,#2889));
#918=EDGE_LOOP('',(#2890,#2891,#2892,#2893));
#919=EDGE_LOOP('',(#2894,#2895,#2896,#2897));
#920=EDGE_LOOP('',(#2898,#2899,#2900,#2901));
#921=EDGE_LOOP('',(#2902,#2903,#2904,#2905));
#922=EDGE_LOOP('',(#2906,#2907,#2908,#2909));
#923=EDGE_LOOP('',(#2910,#2911,#2912,#2913));
#924=EDGE_LOOP('',(#2914,#2915,#2916,#2917));
#925=EDGE_LOOP('',(#2918,#2919,#2920,#2921));
#926=EDGE_LOOP('',(#2922,#2923,#2924,#2925));
#927=EDGE_LOOP('',(#2926,#2927,#2928,#2929));
#928=EDGE_LOOP('',(#2930,#2931,#2932,#2933));
#929=EDGE_LOOP('',(#2934,#2935,#2936,#2937,#2938,#2939,#2940,#2941,#2942,
#2943,#2944,#2945,#2946,#2947,#2948,#2949,#2950,#2951,#2952,#2953,#2954,
#2955,#2956,#2957,#2958,#2959,#2960,#2961,#2962,#2963,#2964,#2965,#2966,
#2967,#2968,#2969,#2970,#2971,#2972,#2973,#2974,#2975,#2976,#2977));
#930=EDGE_LOOP('',(#2978));
#931=EDGE_LOOP('',(#2979,#2980,#2981,#2982,#2983,#2984,#2985,#2986,#2987,
#2988,#2989,#2990,#2991,#2992,#2993,#2994,#2995,#2996,#2997,#2998,#2999,
#3000,#3001,#3002,#3003,#3004,#3005,#3006,#3007,#3008,#3009,#3010,#3011,
#3012,#3013,#3014,#3015,#3016,#3017,#3018,#3019,#3020,#3021,#3022));
#932=EDGE_LOOP('',(#3023));
#933=EDGE_LOOP('',(#3024,#3025,#3026,#3027));
#934=EDGE_LOOP('',(#3028));
#935=EDGE_LOOP('',(#3029,#3030,#3031,#3032));
#936=EDGE_LOOP('',(#3033));
#937=EDGE_LOOP('',(#3034));
#938=EDGE_LOOP('',(#3035));
#939=EDGE_LOOP('',(#3036));
#940=EDGE_LOOP('',(#3037));
#941=EDGE_LOOP('',(#3038,#3039,#3040,#3041));
#942=EDGE_LOOP('',(#3042,#3043,#3044,#3045));
#943=EDGE_LOOP('',(#3046,#3047,#3048,#3049));
#944=EDGE_LOOP('',(#3050));
#945=EDGE_LOOP('',(#3051));
#946=EDGE_LOOP('',(#3052));
#947=EDGE_LOOP('',(#3053));
#948=EDGE_LOOP('',(#3054,#3055,#3056,#3057));
#949=EDGE_LOOP('',(#3058,#3059,#3060,#3061));
#950=EDGE_LOOP('',(#3062,#3063,#3064,#3065));
#951=EDGE_LOOP('',(#3066));
#952=EDGE_LOOP('',(#3067,#3068,#3069,#3070));
#953=EDGE_LOOP('',(#3071,#3072,#3073,#3074));
#954=EDGE_LOOP('',(#3075,#3076,#3077,#3078));
#955=EDGE_LOOP('',(#3079));
#956=EDGE_LOOP('',(#3080,#3081,#3082,#3083,#3084,#3085,#3086,#3087,#3088,
#3089,#3090,#3091));
#957=EDGE_LOOP('',(#3092));
#958=EDGE_LOOP('',(#3093,#3094,#3095,#3096));
#959=EDGE_LOOP('',(#3097,#3098,#3099,#3100));
#960=EDGE_LOOP('',(#3101,#3102,#3103,#3104));
#961=EDGE_LOOP('',(#3105,#3106,#3107,#3108));
#962=EDGE_LOOP('',(#3109,#3110,#3111,#3112));
#963=EDGE_LOOP('',(#3113,#3114,#3115,#3116));
#964=EDGE_LOOP('',(#3117,#3118,#3119,#3120));
#965=EDGE_LOOP('',(#3121,#3122,#3123,#3124));
#966=EDGE_LOOP('',(#3125,#3126,#3127,#3128));
#967=EDGE_LOOP('',(#3129,#3130,#3131,#3132));
#968=EDGE_LOOP('',(#3133,#3134,#3135,#3136,#3137,#3138,#3139,#3140,#3141,
#3142,#3143,#3144));
#969=EDGE_LOOP('',(#3145));
#970=EDGE_LOOP('',(#3146,#3147,#3148,#3149,#3150,#3151,#3152,#3153));
#971=EDGE_LOOP('',(#3154,#3155,#3156,#3157,#3158,#3159,#3160,#3161));
#972=EDGE_LOOP('',(#3162,#3163,#3164,#3165));
#973=EDGE_LOOP('',(#3166));
#974=EDGE_LOOP('',(#3167));
#975=EDGE_LOOP('',(#3168,#3169,#3170,#3171));
#976=EDGE_LOOP('',(#3172,#3173,#3174,#3175));
#977=EDGE_LOOP('',(#3176,#3177,#3178,#3179));
#978=EDGE_LOOP('',(#3180));
#979=EDGE_LOOP('',(#3181,#3182,#3183,#3184));
#980=EDGE_LOOP('',(#3185,#3186,#3187,#3188));
#981=EDGE_LOOP('',(#3189,#3190,#3191,#3192));
#982=EDGE_LOOP('',(#3193));
#983=EDGE_LOOP('',(#3194,#3195,#3196,#3197,#3198,#3199,#3200,#3201,#3202,
#3203,#3204,#3205));
#984=EDGE_LOOP('',(#3206));
#985=EDGE_LOOP('',(#3207,#3208,#3209,#3210));
#986=EDGE_LOOP('',(#3211,#3212,#3213,#3214));
#987=EDGE_LOOP('',(#3215,#3216,#3217,#3218));
#988=EDGE_LOOP('',(#3219,#3220,#3221,#3222));
#989=EDGE_LOOP('',(#3223,#3224,#3225,#3226));
#990=EDGE_LOOP('',(#3227,#3228,#3229,#3230));
#991=EDGE_LOOP('',(#3231,#3232,#3233,#3234));
#992=EDGE_LOOP('',(#3235,#3236,#3237,#3238));
#993=EDGE_LOOP('',(#3239,#3240,#3241,#3242));
#994=EDGE_LOOP('',(#3243,#3244,#3245,#3246));
#995=EDGE_LOOP('',(#3247,#3248,#3249,#3250,#3251,#3252,#3253,#3254,#3255,
#3256,#3257,#3258));
#996=EDGE_LOOP('',(#3259));
#997=EDGE_LOOP('',(#3260,#3261,#3262,#3263,#3264,#3265,#3266,#3267));
#998=EDGE_LOOP('',(#3268,#3269,#3270,#3271,#3272,#3273,#3274,#3275));
#999=EDGE_LOOP('',(#3276,#3277,#3278,#3279));
#1000=EDGE_LOOP('',(#3280));
#1001=EDGE_LOOP('',(#3281));
#1002=EDGE_LOOP('',(#3282,#3283,#3284,#3285));
#1003=EDGE_LOOP('',(#3286,#3287,#3288,#3289));
#1004=EDGE_LOOP('',(#3290,#3291,#3292,#3293));
#1005=EDGE_LOOP('',(#3294,#3295,#3296,#3297));
#1006=EDGE_LOOP('',(#3298,#3299,#3300,#3301));
#1007=EDGE_LOOP('',(#3302,#3303,#3304,#3305));
#1008=EDGE_LOOP('',(#3306,#3307,#3308,#3309,#3310,#3311));
#1009=EDGE_LOOP('',(#3312,#3313,#3314,#3315,#3316,#3317));
#1010=EDGE_LOOP('',(#3318));
#1011=EDGE_LOOP('',(#3319));
#1012=EDGE_LOOP('',(#3320,#3321,#3322,#3323));
#1013=EDGE_LOOP('',(#3324,#3325,#3326,#3327));
#1014=EDGE_LOOP('',(#3328,#3329,#3330,#3331));
#1015=EDGE_LOOP('',(#3332));
#1016=EDGE_LOOP('',(#3333));
#1017=EDGE_LOOP('',(#3334,#3335,#3336,#3337));
#1018=EDGE_LOOP('',(#3338,#3339,#3340,#3341));
#1019=EDGE_LOOP('',(#3342,#3343,#3344,#3345));
#1020=EDGE_LOOP('',(#3346,#3347,#3348,#3349));
#1021=EDGE_LOOP('',(#3350,#3351,#3352,#3353));
#1022=EDGE_LOOP('',(#3354));
#1023=EDGE_LOOP('',(#3355,#3356,#3357,#3358,#3359,#3360,#3361,#3362,#3363,
#3364));
#1024=EDGE_LOOP('',(#3365,#3366,#3367,#3368));
#1025=EDGE_LOOP('',(#3369,#3370,#3371,#3372));
#1026=EDGE_LOOP('',(#3373,#3374,#3375,#3376,#3377,#3378,#3379,#3380,#3381,
#3382));
#1027=EDGE_LOOP('',(#3383,#3384,#3385,#3386));
#1028=EDGE_LOOP('',(#3387,#3388,#3389,#3390,#3391,#3392));
#1029=EDGE_LOOP('',(#3393,#3394,#3395,#3396,#3397,#3398,#3399,#3400));
#1030=EDGE_LOOP('',(#3401,#3402,#3403,#3404,#3405));
#1031=EDGE_LOOP('',(#3406,#3407,#3408,#3409));
#1032=EDGE_LOOP('',(#3410,#3411,#3412,#3413,#3414,#3415));
#1033=EDGE_LOOP('',(#3416,#3417,#3418,#3419));
#1034=EDGE_LOOP('',(#3420,#3421,#3422,#3423,#3424,#3425));
#1035=EDGE_LOOP('',(#3426,#3427,#3428,#3429,#3430));
#1036=EDGE_LOOP('',(#3431,#3432,#3433,#3434));
#1037=EDGE_LOOP('',(#3435,#3436,#3437,#3438));
#1038=EDGE_LOOP('',(#3439));
#1039=EDGE_LOOP('',(#3440));
#1040=EDGE_LOOP('',(#3441,#3442,#3443,#3444,#3445));
#1041=EDGE_LOOP('',(#3446));
#1042=EDGE_LOOP('',(#3447));
#1043=EDGE_LOOP('',(#3448,#3449,#3450,#3451));
#1044=EDGE_LOOP('',(#3452,#3453,#3454,#3455,#3456,#3457));
#1045=EDGE_LOOP('',(#3458,#3459,#3460,#3461,#3462));
#1046=EDGE_LOOP('',(#3463));
#1047=EDGE_LOOP('',(#3464));
#1048=EDGE_LOOP('',(#3465,#3466,#3467,#3468));
#1049=EDGE_LOOP('',(#3469,#3470,#3471,#3472));
#1050=EDGE_LOOP('',(#3473,#3474,#3475,#3476));
#1051=EDGE_LOOP('',(#3477));
#1052=EDGE_LOOP('',(#3478));
#1053=EDGE_LOOP('',(#3479,#3480,#3481,#3482,#3483));
#1054=EDGE_LOOP('',(#3484,#3485));
#1055=EDGE_LOOP('',(#3486,#3487));
#1056=EDGE_LOOP('',(#3488,#3489));
#1057=EDGE_LOOP('',(#3490,#3491));
#1058=EDGE_LOOP('',(#3492,#3493));
#1059=EDGE_LOOP('',(#3494,#3495));
#1060=EDGE_LOOP('',(#3496,#3497));
#1061=EDGE_LOOP('',(#3498,#3499));
#1062=EDGE_LOOP('',(#3500,#3501,#3502,#3503));
#1063=EDGE_LOOP('',(#3504,#3505,#3506,#3507,#3508,#3509,#3510,#3511,#3512,
#3513,#3514,#3515,#3516,#3517,#3518,#3519,#3520,#3521,#3522,#3523));
#1064=EDGE_LOOP('',(#3524,#3525,#3526,#3527));
#1065=EDGE_LOOP('',(#3528,#3529,#3530,#3531));
#1066=EDGE_LOOP('',(#3532,#3533,#3534,#3535));
#1067=EDGE_LOOP('',(#3536,#3537,#3538,#3539));
#1068=EDGE_LOOP('',(#3540,#3541,#3542,#3543));
#1069=EDGE_LOOP('',(#3544,#3545,#3546,#3547,#3548,#3549));
#1070=EDGE_LOOP('',(#3550,#3551,#3552,#3553));
#1071=EDGE_LOOP('',(#3554,#3555,#3556,#3557));
#1072=EDGE_LOOP('',(#3558,#3559,#3560,#3561));
#1073=EDGE_LOOP('',(#3562,#3563,#3564,#3565));
#1074=EDGE_LOOP('',(#3566,#3567,#3568,#3569));
#1075=EDGE_LOOP('',(#3570,#3571,#3572,#3573));
#1076=EDGE_LOOP('',(#3574,#3575,#3576,#3577,#3578,#3579,#3580,#3581,#3582,
#3583,#3584,#3585,#3586,#3587,#3588,#3589,#3590,#3591,#3592,#3593));
#1077=EDGE_LOOP('',(#3594,#3595,#3596,#3597));
#1078=EDGE_LOOP('',(#3598,#3599,#3600,#3601));
#1079=EDGE_LOOP('',(#3602));
#1080=EDGE_LOOP('',(#3603));
#1081=EDGE_LOOP('',(#3604,#3605,#3606,#3607));
#1082=EDGE_LOOP('',(#3608));
#1083=EDGE_LOOP('',(#3609));
#1084=EDGE_LOOP('',(#3610,#3611,#3612,#3613));
#1085=EDGE_LOOP('',(#3614));
#1086=EDGE_LOOP('',(#3615));
#1087=EDGE_LOOP('',(#3616,#3617,#3618,#3619));
#1088=EDGE_LOOP('',(#3620));
#1089=EDGE_LOOP('',(#3621));
#1090=EDGE_LOOP('',(#3622,#3623,#3624,#3625));
#1091=EDGE_LOOP('',(#3626));
#1092=EDGE_LOOP('',(#3627));
#1093=EDGE_LOOP('',(#3628,#3629,#3630,#3631));
#1094=EDGE_LOOP('',(#3632,#3633,#3634,#3635));
#1095=EDGE_LOOP('',(#3636,#3637,#3638,#3639));
#1096=EDGE_LOOP('',(#3640));
#1097=EDGE_LOOP('',(#3641));
#1098=EDGE_LOOP('',(#3642));
#1099=EDGE_LOOP('',(#3643));
#1100=EDGE_LOOP('',(#3644,#3645,#3646,#3647));
#1101=EDGE_LOOP('',(#3648,#3649,#3650,#3651));
#1102=EDGE_LOOP('',(#3652));
#1103=EDGE_LOOP('',(#3653));
#1104=EDGE_LOOP('',(#3654));
#1105=EDGE_LOOP('',(#3655));
#1106=EDGE_LOOP('',(#3656,#3657,#3658,#3659));
#1107=EDGE_LOOP('',(#3660,#3661,#3662,#3663));
#1108=EDGE_LOOP('',(#3664));
#1109=EDGE_LOOP('',(#3665));
#1110=EDGE_LOOP('',(#3666));
#1111=EDGE_LOOP('',(#3667));
#1112=EDGE_LOOP('',(#3668,#3669,#3670,#3671));
#1113=EDGE_LOOP('',(#3672,#3673,#3674,#3675));
#1114=EDGE_LOOP('',(#3676));
#1115=EDGE_LOOP('',(#3677));
#1116=EDGE_LOOP('',(#3678));
#1117=EDGE_LOOP('',(#3679));
#1118=EDGE_LOOP('',(#3680,#3681,#3682,#3683));
#1119=EDGE_LOOP('',(#3684,#3685,#3686,#3687));
#1120=EDGE_LOOP('',(#3688,#3689,#3690,#3691));
#1121=EDGE_LOOP('',(#3692,#3693,#3694,#3695));
#1122=EDGE_LOOP('',(#3696,#3697,#3698,#3699));
#1123=EDGE_LOOP('',(#3700));
#1124=EDGE_LOOP('',(#3701));
#1125=EDGE_LOOP('',(#3702,#3703,#3704,#3705));
#1126=EDGE_LOOP('',(#3706,#3707,#3708,#3709));
#1127=EDGE_LOOP('',(#3710));
#1128=EDGE_LOOP('',(#3711));
#1129=EDGE_LOOP('',(#3712));
#1130=EDGE_LOOP('',(#3713));
#1131=EDGE_LOOP('',(#3714));
#1132=EDGE_LOOP('',(#3715));
#1133=EDGE_LOOP('',(#3716));
#1134=EDGE_LOOP('',(#3717));
#1135=EDGE_LOOP('',(#3718));
#1136=EDGE_LOOP('',(#3719));
#1137=EDGE_LOOP('',(#3720));
#1138=EDGE_LOOP('',(#3721));
#1139=EDGE_LOOP('',(#3722,#3723,#3724,#3725));
#1140=EDGE_LOOP('',(#3726,#3727,#3728,#3729));
#1141=EDGE_LOOP('',(#3730,#3731,#3732,#3733));
#1142=EDGE_LOOP('',(#3734,#3735,#3736,#3737));
#1143=EDGE_LOOP('',(#3738,#3739,#3740,#3741));
#1144=EDGE_LOOP('',(#3742,#3743,#3744,#3745));
#1145=EDGE_LOOP('',(#3746));
#1146=EDGE_LOOP('',(#3747));
#1147=EDGE_LOOP('',(#3748));
#1148=EDGE_LOOP('',(#3749));
#1149=EDGE_LOOP('',(#3750));
#1150=EDGE_LOOP('',(#3751));
#1151=EDGE_LOOP('',(#3752));
#1152=EDGE_LOOP('',(#3753));
#1153=EDGE_LOOP('',(#3754));
#1154=EDGE_LOOP('',(#3755));
#1155=EDGE_LOOP('',(#3756));
#1156=EDGE_LOOP('',(#3757));
#1157=EDGE_LOOP('',(#3758));
#1158=EDGE_LOOP('',(#3759,#3760,#3761,#3762));
#1159=EDGE_LOOP('',(#3763,#3764,#3765,#3766));
#1160=EDGE_LOOP('',(#3767,#3768,#3769,#3770));
#1161=EDGE_LOOP('',(#3771));
#1162=EDGE_LOOP('',(#3772));
#1163=EDGE_LOOP('',(#3773,#3774,#3775,#3776));
#1164=EDGE_LOOP('',(#3777,#3778,#3779,#3780));
#1165=EDGE_LOOP('',(#3781,#3782,#3783,#3784));
#1166=EDGE_LOOP('',(#3785));
#1167=EDGE_LOOP('',(#3786,#3787,#3788,#3789));
#1168=EDGE_LOOP('',(#3790,#3791,#3792,#3793));
#1169=EDGE_LOOP('',(#3794,#3795,#3796,#3797));
#1170=EDGE_LOOP('',(#3798,#3799,#3800,#3801));
#1171=EDGE_LOOP('',(#3802,#3803,#3804,#3805));
#1172=EDGE_LOOP('',(#3806,#3807,#3808,#3809));
#1173=EDGE_LOOP('',(#3810,#3811,#3812,#3813,#3814,#3815));
#1174=EDGE_LOOP('',(#3816,#3817,#3818,#3819,#3820,#3821));
#1175=LINE('',#6222,#1516);
#1176=LINE('',#6224,#1517);
#1177=LINE('',#6226,#1518);
#1178=LINE('',#6227,#1519);
#1179=LINE('',#6230,#1520);
#1180=LINE('',#6232,#1521);
#1181=LINE('',#6233,#1522);
#1182=LINE('',#6236,#1523);
#1183=LINE('',#6238,#1524);
#1184=LINE('',#6239,#1525);
#1185=LINE('',#6242,#1526);
#1186=LINE('',#6244,#1527);
#1187=LINE('',#6245,#1528);
#1188=LINE('',#6248,#1529);
#1189=LINE('',#6250,#1530);
#1190=LINE('',#6251,#1531);
#1191=LINE('',#6254,#1532);
#1192=LINE('',#6256,#1533);
#1193=LINE('',#6257,#1534);
#1194=LINE('',#6260,#1535);
#1195=LINE('',#6262,#1536);
#1196=LINE('',#6263,#1537);
#1197=LINE('',#6266,#1538);
#1198=LINE('',#6268,#1539);
#1199=LINE('',#6269,#1540);
#1200=LINE('',#6272,#1541);
#1201=LINE('',#6274,#1542);
#1202=LINE('',#6275,#1543);
#1203=LINE('',#6279,#1544);
#1204=LINE('',#6281,#1545);
#1205=LINE('',#6283,#1546);
#1206=LINE('',#6284,#1547);
#1207=LINE('',#6287,#1548);
#1208=LINE('',#6289,#1549);
#1209=LINE('',#6290,#1550);
#1210=LINE('',#6293,#1551);
#1211=LINE('',#6295,#1552);
#1212=LINE('',#6296,#1553);
#1213=LINE('',#6299,#1554);
#1214=LINE('',#6301,#1555);
#1215=LINE('',#6302,#1556);
#1216=LINE('',#6305,#1557);
#1217=LINE('',#6307,#1558);
#1218=LINE('',#6308,#1559);
#1219=LINE('',#6311,#1560);
#1220=LINE('',#6313,#1561);
#1221=LINE('',#6314,#1562);
#1222=LINE('',#6317,#1563);
#1223=LINE('',#6319,#1564);
#1224=LINE('',#6320,#1565);
#1225=LINE('',#6323,#1566);
#1226=LINE('',#6325,#1567);
#1227=LINE('',#6326,#1568);
#1228=LINE('',#6329,#1569);
#1229=LINE('',#6331,#1570);
#1230=LINE('',#6332,#1571);
#1231=LINE('',#6336,#1572);
#1232=LINE('',#6338,#1573);
#1233=LINE('',#6340,#1574);
#1234=LINE('',#6341,#1575);
#1235=LINE('',#6344,#1576);
#1236=LINE('',#6346,#1577);
#1237=LINE('',#6347,#1578);
#1238=LINE('',#6350,#1579);
#1239=LINE('',#6352,#1580);
#1240=LINE('',#6353,#1581);
#1241=LINE('',#6356,#1582);
#1242=LINE('',#6358,#1583);
#1243=LINE('',#6359,#1584);
#1244=LINE('',#6362,#1585);
#1245=LINE('',#6364,#1586);
#1246=LINE('',#6365,#1587);
#1247=LINE('',#6368,#1588);
#1248=LINE('',#6370,#1589);
#1249=LINE('',#6371,#1590);
#1250=LINE('',#6374,#1591);
#1251=LINE('',#6376,#1592);
#1252=LINE('',#6377,#1593);
#1253=LINE('',#6380,#1594);
#1254=LINE('',#6382,#1595);
#1255=LINE('',#6383,#1596);
#1256=LINE('',#6386,#1597);
#1257=LINE('',#6388,#1598);
#1258=LINE('',#6389,#1599);
#1259=LINE('',#6393,#1600);
#1260=LINE('',#6395,#1601);
#1261=LINE('',#6397,#1602);
#1262=LINE('',#6398,#1603);
#1263=LINE('',#6401,#1604);
#1264=LINE('',#6403,#1605);
#1265=LINE('',#6404,#1606);
#1266=LINE('',#6407,#1607);
#1267=LINE('',#6409,#1608);
#1268=LINE('',#6410,#1609);
#1269=LINE('',#6413,#1610);
#1270=LINE('',#6415,#1611);
#1271=LINE('',#6416,#1612);
#1272=LINE('',#6419,#1613);
#1273=LINE('',#6421,#1614);
#1274=LINE('',#6422,#1615);
#1275=LINE('',#6425,#1616);
#1276=LINE('',#6427,#1617);
#1277=LINE('',#6428,#1618);
#1278=LINE('',#6431,#1619);
#1279=LINE('',#6433,#1620);
#1280=LINE('',#6434,#1621);
#1281=LINE('',#6437,#1622);
#1282=LINE('',#6439,#1623);
#1283=LINE('',#6440,#1624);
#1284=LINE('',#6443,#1625);
#1285=LINE('',#6445,#1626);
#1286=LINE('',#6446,#1627);
#1287=LINE('',#6451,#1628);
#1288=LINE('',#6455,#1629);
#1289=LINE('',#6457,#1630);
#1290=LINE('',#6458,#1631);
#1291=LINE('',#6461,#1632);
#1292=LINE('',#6463,#1633);
#1293=LINE('',#6464,#1634);
#1294=LINE('',#6466,#1635);
#1295=LINE('',#6467,#1636);
#1296=LINE('',#6470,#1637);
#1297=LINE('',#6472,#1638);
#1298=LINE('',#6473,#1639);
#1299=LINE('',#6475,#1640);
#1300=LINE('',#6476,#1641);
#1301=LINE('',#6479,#1642);
#1302=LINE('',#6481,#1643);
#1303=LINE('',#6482,#1644);
#1304=LINE('',#6484,#1645);
#1305=LINE('',#6485,#1646);
#1306=LINE('',#6487,#1647);
#1307=LINE('',#6488,#1648);
#1308=LINE('',#6497,#1649);
#1309=LINE('',#6504,#1650);
#1310=LINE('',#6518,#1651);
#1311=LINE('',#6521,#1652);
#1312=LINE('',#6526,#1653);
#1313=LINE('',#6533,#1654);
#1314=LINE('',#6537,#1655);
#1315=LINE('',#6542,#1656);
#1316=LINE('',#6546,#1657);
#1317=LINE('',#6549,#1658);
#1318=LINE('',#6550,#1659);
#1319=LINE('',#6556,#1660);
#1320=LINE('',#6560,#1661);
#1321=LINE('',#6565,#1662);
#1322=LINE('',#6569,#1663);
#1323=LINE('',#6572,#1664);
#1324=LINE('',#6573,#1665);
#1325=LINE('',#6578,#1666);
#1326=LINE('',#6580,#1667);
#1327=LINE('',#6582,#1668);
#1328=LINE('',#6584,#1669);
#1329=LINE('',#6585,#1670);
#1330=LINE('',#6586,#1671);
#1331=LINE('',#6591,#1672);
#1332=LINE('',#6592,#1673);
#1333=LINE('',#6595,#1674);
#1334=LINE('',#6596,#1675);
#1335=LINE('',#6598,#1676);
#1336=LINE('',#6602,#1677);
#1337=LINE('',#6606,#1678);
#1338=LINE('',#6609,#1679);
#1339=LINE('',#6613,#1680);
#1340=LINE('',#6615,#1681);
#1341=LINE('',#6616,#1682);
#1342=LINE('',#6620,#1683);
#1343=LINE('',#6622,#1684);
#1344=LINE('',#6624,#1685);
#1345=LINE('',#6625,#1686);
#1346=LINE('',#6628,#1687);
#1347=LINE('',#6630,#1688);
#1348=LINE('',#6631,#1689);
#1349=LINE('',#6634,#1690);
#1350=LINE('',#6636,#1691);
#1351=LINE('',#6637,#1692);
#1352=LINE('',#6639,#1693);
#1353=LINE('',#6640,#1694);
#1354=LINE('',#6642,#1695);
#1355=LINE('',#6644,#1696);
#1356=LINE('',#6650,#1697);
#1357=LINE('',#6654,#1698);
#1358=LINE('',#6659,#1699);
#1359=LINE('',#6663,#1700);
#1360=LINE('',#6666,#1701);
#1361=LINE('',#6667,#1702);
#1362=LINE('',#6673,#1703);
#1363=LINE('',#6677,#1704);
#1364=LINE('',#6682,#1705);
#1365=LINE('',#6686,#1706);
#1366=LINE('',#6689,#1707);
#1367=LINE('',#6690,#1708);
#1368=LINE('',#6695,#1709);
#1369=LINE('',#6697,#1710);
#1370=LINE('',#6699,#1711);
#1371=LINE('',#6701,#1712);
#1372=LINE('',#6702,#1713);
#1373=LINE('',#6703,#1714);
#1374=LINE('',#6708,#1715);
#1375=LINE('',#6709,#1716);
#1376=LINE('',#6712,#1717);
#1377=LINE('',#6713,#1718);
#1378=LINE('',#6715,#1719);
#1379=LINE('',#6719,#1720);
#1380=LINE('',#6723,#1721);
#1381=LINE('',#6726,#1722);
#1382=LINE('',#6730,#1723);
#1383=LINE('',#6732,#1724);
#1384=LINE('',#6733,#1725);
#1385=LINE('',#6737,#1726);
#1386=LINE('',#6739,#1727);
#1387=LINE('',#6741,#1728);
#1388=LINE('',#6742,#1729);
#1389=LINE('',#6745,#1730);
#1390=LINE('',#6747,#1731);
#1391=LINE('',#6748,#1732);
#1392=LINE('',#6751,#1733);
#1393=LINE('',#6753,#1734);
#1394=LINE('',#6754,#1735);
#1395=LINE('',#6756,#1736);
#1396=LINE('',#6757,#1737);
#1397=LINE('',#6759,#1738);
#1398=LINE('',#6761,#1739);
#1399=LINE('',#6767,#1740);
#1400=LINE('',#6769,#1741);
#1401=LINE('',#6771,#1742);
#1402=LINE('',#6772,#1743);
#1403=LINE('',#6775,#1744);
#1404=LINE('',#6777,#1745);
#1405=LINE('',#6778,#1746);
#1406=LINE('',#6781,#1747);
#1407=LINE('',#6783,#1748);
#1408=LINE('',#6784,#1749);
#1409=LINE('',#6787,#1750);
#1410=LINE('',#6789,#1751);
#1411=LINE('',#6790,#1752);
#1412=LINE('',#6793,#1753);
#1413=LINE('',#6795,#1754);
#1414=LINE('',#6796,#1755);
#1415=LINE('',#6798,#1756);
#1416=LINE('',#6799,#1757);
#1417=LINE('',#6811,#1758);
#1418=LINE('',#6815,#1759);
#1419=LINE('',#6819,#1760);
#1420=LINE('',#6826,#1761);
#1421=LINE('',#6828,#1762);
#1422=LINE('',#6833,#1763);
#1423=LINE('',#6835,#1764);
#1424=LINE('',#6837,#1765);
#1425=LINE('',#6838,#1766);
#1426=LINE('',#6841,#1767);
#1427=LINE('',#6843,#1768);
#1428=LINE('',#6844,#1769);
#1429=LINE('',#6847,#1770);
#1430=LINE('',#6849,#1771);
#1431=LINE('',#6850,#1772);
#1432=LINE('',#6855,#1773);
#1433=LINE('',#6857,#1774);
#1434=LINE('',#6859,#1775);
#1435=LINE('',#6861,#1776);
#1436=LINE('',#6863,#1777);
#1437=LINE('',#6865,#1778);
#1438=LINE('',#6866,#1779);
#1439=LINE('',#6869,#1780);
#1440=LINE('',#6870,#1781);
#1441=LINE('',#6873,#1782);
#1442=LINE('',#6874,#1783);
#1443=LINE('',#6877,#1784);
#1444=LINE('',#6879,#1785);
#1445=LINE('',#6881,#1786);
#1446=LINE('',#6883,#1787);
#1447=LINE('',#6884,#1788);
#1448=LINE('',#6886,#1789);
#1449=LINE('',#6889,#1790);
#1450=LINE('',#6892,#1791);
#1451=LINE('',#6896,#1792);
#1452=LINE('',#6903,#1793);
#1453=LINE('',#6905,#1794);
#1454=LINE('',#6907,#1795);
#1455=LINE('',#6923,#1796);
#1456=LINE('',#6929,#1797);
#1457=LINE('',#6933,#1798);
#1458=LINE('',#6939,#1799);
#1459=LINE('',#6944,#1800);
#1460=LINE('',#6959,#1801);
#1461=LINE('',#6968,#1802);
#1462=LINE('',#6972,#1803);
#1463=LINE('',#6976,#1804);
#1464=LINE('',#6979,#1805);
#1465=LINE('',#7132,#1806);
#1466=LINE('',#7428,#1807);
#1467=LINE('',#7470,#1808);
#1468=LINE('',#7475,#1809);
#1469=LINE('',#7484,#1810);
#1470=LINE('',#7489,#1811);
#1471=LINE('',#7500,#1812);
#1472=LINE('',#7506,#1813);
#1473=LINE('',#7515,#1814);
#1474=LINE('',#7521,#1815);
#1475=LINE('',#7530,#1816);
#1476=LINE('',#7536,#1817);
#1477=LINE('',#7546,#1818);
#1478=LINE('',#7552,#1819);
#1479=LINE('',#7561,#1820);
#1480=LINE('',#7567,#1821);
#1481=LINE('',#7573,#1822);
#1482=LINE('',#7579,#1823);
#1483=LINE('',#7585,#1824);
#1484=LINE('',#7592,#1825);
#1485=LINE('',#7598,#1826);
#1486=LINE('',#7607,#1827);
#1487=LINE('',#7613,#1828);
#1488=LINE('',#7619,#1829);
#1489=LINE('',#7625,#1830);
#1490=LINE('',#7631,#1831);
#1491=LINE('',#7637,#1832);
#1492=LINE('',#7648,#1833);
#1493=LINE('',#7652,#1834);
#1494=LINE('',#7656,#1835);
#1495=LINE('',#7663,#1836);
#1496=LINE('',#7667,#1837);
#1497=LINE('',#7671,#1838);
#1498=LINE('',#7676,#1839);
#1499=LINE('',#7678,#1840);
#1500=LINE('',#7680,#1841);
#1501=LINE('',#7681,#1842);
#1502=LINE('',#7684,#1843);
#1503=LINE('',#7686,#1844);
#1504=LINE('',#7687,#1845);
#1505=LINE('',#7690,#1846);
#1506=LINE('',#7692,#1847);
#1507=LINE('',#7693,#1848);
#1508=LINE('',#7696,#1849);
#1509=LINE('',#7698,#1850);
#1510=LINE('',#7699,#1851);
#1511=LINE('',#7702,#1852);
#1512=LINE('',#7704,#1853);
#1513=LINE('',#7705,#1854);
#1514=LINE('',#7707,#1855);
#1515=LINE('',#7708,#1856);
#1516=VECTOR('',#4917,1.);
#1517=VECTOR('',#4918,1.);
#1518=VECTOR('',#4919,1.);
#1519=VECTOR('',#4920,1.);
#1520=VECTOR('',#4923,1.);
#1521=VECTOR('',#4924,1.);
#1522=VECTOR('',#4925,1.);
#1523=VECTOR('',#4928,1.);
#1524=VECTOR('',#4929,1.);
#1525=VECTOR('',#4930,1.);
#1526=VECTOR('',#4933,1.);
#1527=VECTOR('',#4934,1.);
#1528=VECTOR('',#4935,1.);
#1529=VECTOR('',#4938,1.);
#1530=VECTOR('',#4939,1.);
#1531=VECTOR('',#4940,1.);
#1532=VECTOR('',#4943,1.);
#1533=VECTOR('',#4944,1.);
#1534=VECTOR('',#4945,1.);
#1535=VECTOR('',#4948,1.);
#1536=VECTOR('',#4949,1.);
#1537=VECTOR('',#4950,1.);
#1538=VECTOR('',#4953,1.);
#1539=VECTOR('',#4954,1.);
#1540=VECTOR('',#4955,1.);
#1541=VECTOR('',#4958,1.);
#1542=VECTOR('',#4959,1.);
#1543=VECTOR('',#4960,1.);
#1544=VECTOR('',#4963,1.);
#1545=VECTOR('',#4964,1.);
#1546=VECTOR('',#4965,1.);
#1547=VECTOR('',#4966,1.);
#1548=VECTOR('',#4969,1.);
#1549=VECTOR('',#4970,1.);
#1550=VECTOR('',#4971,1.);
#1551=VECTOR('',#4974,1.);
#1552=VECTOR('',#4975,1.);
#1553=VECTOR('',#4976,1.);
#1554=VECTOR('',#4979,1.);
#1555=VECTOR('',#4980,1.);
#1556=VECTOR('',#4981,1.);
#1557=VECTOR('',#4984,1.);
#1558=VECTOR('',#4985,1.);
#1559=VECTOR('',#4986,1.);
#1560=VECTOR('',#4989,1.);
#1561=VECTOR('',#4990,1.);
#1562=VECTOR('',#4991,1.);
#1563=VECTOR('',#4994,1.);
#1564=VECTOR('',#4995,1.);
#1565=VECTOR('',#4996,1.);
#1566=VECTOR('',#4999,1.);
#1567=VECTOR('',#5000,1.);
#1568=VECTOR('',#5001,1.);
#1569=VECTOR('',#5004,1.);
#1570=VECTOR('',#5005,1.);
#1571=VECTOR('',#5006,1.);
#1572=VECTOR('',#5009,1.);
#1573=VECTOR('',#5010,1.);
#1574=VECTOR('',#5011,1.);
#1575=VECTOR('',#5012,1.);
#1576=VECTOR('',#5015,1.);
#1577=VECTOR('',#5016,1.);
#1578=VECTOR('',#5017,1.);
#1579=VECTOR('',#5020,1.);
#1580=VECTOR('',#5021,1.);
#1581=VECTOR('',#5022,1.);
#1582=VECTOR('',#5025,1.);
#1583=VECTOR('',#5026,1.);
#1584=VECTOR('',#5027,1.);
#1585=VECTOR('',#5030,1.);
#1586=VECTOR('',#5031,1.);
#1587=VECTOR('',#5032,1.);
#1588=VECTOR('',#5035,1.);
#1589=VECTOR('',#5036,1.);
#1590=VECTOR('',#5037,1.);
#1591=VECTOR('',#5040,1.);
#1592=VECTOR('',#5041,1.);
#1593=VECTOR('',#5042,1.);
#1594=VECTOR('',#5045,1.);
#1595=VECTOR('',#5046,1.);
#1596=VECTOR('',#5047,1.);
#1597=VECTOR('',#5050,1.);
#1598=VECTOR('',#5051,1.);
#1599=VECTOR('',#5052,1.);
#1600=VECTOR('',#5055,1.);
#1601=VECTOR('',#5056,1.);
#1602=VECTOR('',#5057,1.);
#1603=VECTOR('',#5058,1.);
#1604=VECTOR('',#5061,1.);
#1605=VECTOR('',#5062,1.);
#1606=VECTOR('',#5063,1.);
#1607=VECTOR('',#5066,1.);
#1608=VECTOR('',#5067,1.);
#1609=VECTOR('',#5068,1.);
#1610=VECTOR('',#5071,1.);
#1611=VECTOR('',#5072,1.);
#1612=VECTOR('',#5073,1.);
#1613=VECTOR('',#5076,1.);
#1614=VECTOR('',#5077,1.);
#1615=VECTOR('',#5078,1.);
#1616=VECTOR('',#5081,1.);
#1617=VECTOR('',#5082,1.);
#1618=VECTOR('',#5083,1.);
#1619=VECTOR('',#5086,1.);
#1620=VECTOR('',#5087,1.);
#1621=VECTOR('',#5088,1.);
#1622=VECTOR('',#5091,1.);
#1623=VECTOR('',#5092,1.);
#1624=VECTOR('',#5093,1.);
#1625=VECTOR('',#5096,1.);
#1626=VECTOR('',#5097,1.);
#1627=VECTOR('',#5098,1.);
#1628=VECTOR('',#5103,0.21);
#1629=VECTOR('',#5108,1.);
#1630=VECTOR('',#5109,1.);
#1631=VECTOR('',#5110,1.);
#1632=VECTOR('',#5113,1.);
#1633=VECTOR('',#5114,1.);
#1634=VECTOR('',#5115,1.);
#1635=VECTOR('',#5118,1.);
#1636=VECTOR('',#5119,1.);
#1637=VECTOR('',#5122,1.);
#1638=VECTOR('',#5123,1.);
#1639=VECTOR('',#5124,1.);
#1640=VECTOR('',#5127,1.);
#1641=VECTOR('',#5128,1.);
#1642=VECTOR('',#5131,1.);
#1643=VECTOR('',#5132,1.);
#1644=VECTOR('',#5133,1.);
#1645=VECTOR('',#5136,1.);
#1646=VECTOR('',#5137,1.);
#1647=VECTOR('',#5140,1.);
#1648=VECTOR('',#5141,1.);
#1649=VECTOR('',#5154,0.165);
#1650=VECTOR('',#5163,0.165);
#1651=VECTOR('',#5182,0.6);
#1652=VECTOR('',#5185,0.5);
#1653=VECTOR('',#5192,0.5);
#1654=VECTOR('',#5201,1.);
#1655=VECTOR('',#5204,1.);
#1656=VECTOR('',#5209,1.);
#1657=VECTOR('',#5212,1.);
#1658=VECTOR('',#5217,1.);
#1659=VECTOR('',#5218,1.);
#1660=VECTOR('',#5223,1.);
#1661=VECTOR('',#5226,1.);
#1662=VECTOR('',#5231,1.);
#1663=VECTOR('',#5234,1.);
#1664=VECTOR('',#5239,1.);
#1665=VECTOR('',#5240,1.);
#1666=VECTOR('',#5245,1.);
#1667=VECTOR('',#5246,1.);
#1668=VECTOR('',#5247,1.);
#1669=VECTOR('',#5248,1.);
#1670=VECTOR('',#5249,1.);
#1671=VECTOR('',#5250,1.);
#1672=VECTOR('',#5255,1.);
#1673=VECTOR('',#5256,1.);
#1674=VECTOR('',#5259,1.);
#1675=VECTOR('',#5260,1.);
#1676=VECTOR('',#5263,1.);
#1677=VECTOR('',#5268,0.275);
#1678=VECTOR('',#5273,0.275);
#1679=VECTOR('',#5276,0.505);
#1680=VECTOR('',#5281,1.);
#1681=VECTOR('',#5282,1.);
#1682=VECTOR('',#5283,1.);
#1683=VECTOR('',#5286,1.);
#1684=VECTOR('',#5287,1.);
#1685=VECTOR('',#5288,1.);
#1686=VECTOR('',#5289,1.);
#1687=VECTOR('',#5292,1.);
#1688=VECTOR('',#5293,1.);
#1689=VECTOR('',#5294,1.);
#1690=VECTOR('',#5297,1.);
#1691=VECTOR('',#5298,1.);
#1692=VECTOR('',#5299,1.);
#1693=VECTOR('',#5302,1.);
#1694=VECTOR('',#5303,1.);
#1695=VECTOR('',#5306,1.);
#1696=VECTOR('',#5309,1.);
#1697=VECTOR('',#5316,1.);
#1698=VECTOR('',#5319,1.);
#1699=VECTOR('',#5324,1.);
#1700=VECTOR('',#5327,1.);
#1701=VECTOR('',#5332,1.);
#1702=VECTOR('',#5333,1.);
#1703=VECTOR('',#5338,1.);
#1704=VECTOR('',#5341,1.);
#1705=VECTOR('',#5346,1.);
#1706=VECTOR('',#5349,1.);
#1707=VECTOR('',#5354,1.);
#1708=VECTOR('',#5355,1.);
#1709=VECTOR('',#5360,1.);
#1710=VECTOR('',#5361,1.);
#1711=VECTOR('',#5362,1.);
#1712=VECTOR('',#5363,1.);
#1713=VECTOR('',#5364,1.);
#1714=VECTOR('',#5365,1.);
#1715=VECTOR('',#5370,1.);
#1716=VECTOR('',#5371,1.);
#1717=VECTOR('',#5374,1.);
#1718=VECTOR('',#5375,1.);
#1719=VECTOR('',#5378,1.);
#1720=VECTOR('',#5383,0.275);
#1721=VECTOR('',#5388,0.275);
#1722=VECTOR('',#5391,0.505);
#1723=VECTOR('',#5396,1.);
#1724=VECTOR('',#5397,1.);
#1725=VECTOR('',#5398,1.);
#1726=VECTOR('',#5401,1.);
#1727=VECTOR('',#5402,1.);
#1728=VECTOR('',#5403,1.);
#1729=VECTOR('',#5404,1.);
#1730=VECTOR('',#5407,1.);
#1731=VECTOR('',#5408,1.);
#1732=VECTOR('',#5409,1.);
#1733=VECTOR('',#5412,1.);
#1734=VECTOR('',#5413,1.);
#1735=VECTOR('',#5414,1.);
#1736=VECTOR('',#5417,1.);
#1737=VECTOR('',#5418,1.);
#1738=VECTOR('',#5421,1.);
#1739=VECTOR('',#5424,1.);
#1740=VECTOR('',#5431,1.);
#1741=VECTOR('',#5432,1.);
#1742=VECTOR('',#5433,1.);
#1743=VECTOR('',#5434,1.);
#1744=VECTOR('',#5437,1.);
#1745=VECTOR('',#5438,1.);
#1746=VECTOR('',#5439,1.);
#1747=VECTOR('',#5442,1.);
#1748=VECTOR('',#5443,1.);
#1749=VECTOR('',#5444,1.);
#1750=VECTOR('',#5447,1.);
#1751=VECTOR('',#5448,1.);
#1752=VECTOR('',#5449,1.);
#1753=VECTOR('',#5452,1.);
#1754=VECTOR('',#5453,1.);
#1755=VECTOR('',#5454,1.);
#1756=VECTOR('',#5457,1.);
#1757=VECTOR('',#5458,1.);
#1758=VECTOR('',#5475,0.4);
#1759=VECTOR('',#5480,0.425);
#1760=VECTOR('',#5485,0.41);
#1761=VECTOR('',#5494,0.26);
#1762=VECTOR('',#5497,0.25);
#1763=VECTOR('',#5502,1.);
#1764=VECTOR('',#5503,1.);
#1765=VECTOR('',#5504,1.);
#1766=VECTOR('',#5505,1.);
#1767=VECTOR('',#5508,1.);
#1768=VECTOR('',#5509,1.);
#1769=VECTOR('',#5510,1.);
#1770=VECTOR('',#5513,1.);
#1771=VECTOR('',#5514,1.);
#1772=VECTOR('',#5515,1.);
#1773=VECTOR('',#5520,1.);
#1774=VECTOR('',#5521,1.);
#1775=VECTOR('',#5522,1.);
#1776=VECTOR('',#5523,1.);
#1777=VECTOR('',#5524,1.);
#1778=VECTOR('',#5525,1.);
#1779=VECTOR('',#5526,1.);
#1780=VECTOR('',#5529,1.);
#1781=VECTOR('',#5530,1.);
#1782=VECTOR('',#5533,1.);
#1783=VECTOR('',#5534,1.);
#1784=VECTOR('',#5537,1.);
#1785=VECTOR('',#5538,1.);
#1786=VECTOR('',#5539,1.);
#1787=VECTOR('',#5540,1.);
#1788=VECTOR('',#5541,1.);
#1789=VECTOR('',#5544,1.);
#1790=VECTOR('',#5547,1.);
#1791=VECTOR('',#5550,1.);
#1792=VECTOR('',#5555,0.21);
#1793=VECTOR('',#5564,1.);
#1794=VECTOR('',#5567,1.);
#1795=VECTOR('',#5570,1.);
#1796=VECTOR('',#5591,0.976185);
#1797=VECTOR('',#5598,0.5);
#1798=VECTOR('',#5603,0.53);
#1799=VECTOR('',#5612,0.976185);
#1800=VECTOR('',#5619,0.53);
#1801=VECTOR('',#5638,1.023815);
#1802=VECTOR('',#5649,1.47);
#1803=VECTOR('',#5654,1.5);
#1804=VECTOR('',#5659,1.47);
#1805=VECTOR('',#5664,1.023815);
#1806=VECTOR('',#5715,1.019052);
#1807=VECTOR('',#5792,0.980948);
#1808=VECTOR('',#5821,1.013815);
#1809=VECTOR('',#5828,0.991185);
#1810=VECTOR('',#5839,1.013815);
#1811=VECTOR('',#5846,0.991185);
#1812=VECTOR('',#5863,0.225);
#1813=VECTOR('',#5870,1.1);
#1814=VECTOR('',#5883,0.505);
#1815=VECTOR('',#5890,0.8);
#1816=VECTOR('',#5903,0.605);
#1817=VECTOR('',#5910,1.);
#1818=VECTOR('',#5925,2.2);
#1819=VECTOR('',#5932,2.5);
#1820=VECTOR('',#5945,0.165);
#1821=VECTOR('',#5952,0.165);
#1822=VECTOR('',#5959,0.165);
#1823=VECTOR('',#5966,0.165);
#1824=VECTOR('',#5973,1.2);
#1825=VECTOR('',#5982,1.5);
#1826=VECTOR('',#5989,2.2);
#1827=VECTOR('',#6002,0.225);
#1828=VECTOR('',#6009,0.225);
#1829=VECTOR('',#6016,0.225);
#1830=VECTOR('',#6023,0.225);
#1831=VECTOR('',#6030,1.2);
#1832=VECTOR('',#6037,2.5);
#1833=VECTOR('',#6054,0.325);
#1834=VECTOR('',#6059,0.35);
#1835=VECTOR('',#6064,0.335);
#1836=VECTOR('',#6073,0.21);
#1837=VECTOR('',#6078,0.2);
#1838=VECTOR('',#6083,0.18);
#1839=VECTOR('',#6088,1.);
#1840=VECTOR('',#6089,1.);
#1841=VECTOR('',#6090,1.);
#1842=VECTOR('',#6091,1.);
#1843=VECTOR('',#6094,1.);
#1844=VECTOR('',#6095,1.);
#1845=VECTOR('',#6096,1.);
#1846=VECTOR('',#6099,1.);
#1847=VECTOR('',#6100,1.);
#1848=VECTOR('',#6101,1.);
#1849=VECTOR('',#6104,1.);
#1850=VECTOR('',#6105,1.);
#1851=VECTOR('',#6106,1.);
#1852=VECTOR('',#6109,1.);
#1853=VECTOR('',#6110,1.);
#1854=VECTOR('',#6111,1.);
#1855=VECTOR('',#6114,1.);
#1856=VECTOR('',#6115,1.);
#1857=VERTEX_POINT('',#6220);
#1858=VERTEX_POINT('',#6221);
#1859=VERTEX_POINT('',#6223);
#1860=VERTEX_POINT('',#6225);
#1861=VERTEX_POINT('',#6229);
#1862=VERTEX_POINT('',#6231);
#1863=VERTEX_POINT('',#6235);
#1864=VERTEX_POINT('',#6237);
#1865=VERTEX_POINT('',#6241);
#1866=VERTEX_POINT('',#6243);
#1867=VERTEX_POINT('',#6247);
#1868=VERTEX_POINT('',#6249);
#1869=VERTEX_POINT('',#6253);
#1870=VERTEX_POINT('',#6255);
#1871=VERTEX_POINT('',#6259);
#1872=VERTEX_POINT('',#6261);
#1873=VERTEX_POINT('',#6265);
#1874=VERTEX_POINT('',#6267);
#1875=VERTEX_POINT('',#6271);
#1876=VERTEX_POINT('',#6273);
#1877=VERTEX_POINT('',#6277);
#1878=VERTEX_POINT('',#6278);
#1879=VERTEX_POINT('',#6280);
#1880=VERTEX_POINT('',#6282);
#1881=VERTEX_POINT('',#6286);
#1882=VERTEX_POINT('',#6288);
#1883=VERTEX_POINT('',#6292);
#1884=VERTEX_POINT('',#6294);
#1885=VERTEX_POINT('',#6298);
#1886=VERTEX_POINT('',#6300);
#1887=VERTEX_POINT('',#6304);
#1888=VERTEX_POINT('',#6306);
#1889=VERTEX_POINT('',#6310);
#1890=VERTEX_POINT('',#6312);
#1891=VERTEX_POINT('',#6316);
#1892=VERTEX_POINT('',#6318);
#1893=VERTEX_POINT('',#6322);
#1894=VERTEX_POINT('',#6324);
#1895=VERTEX_POINT('',#6328);
#1896=VERTEX_POINT('',#6330);
#1897=VERTEX_POINT('',#6334);
#1898=VERTEX_POINT('',#6335);
#1899=VERTEX_POINT('',#6337);
#1900=VERTEX_POINT('',#6339);
#1901=VERTEX_POINT('',#6343);
#1902=VERTEX_POINT('',#6345);
#1903=VERTEX_POINT('',#6349);
#1904=VERTEX_POINT('',#6351);
#1905=VERTEX_POINT('',#6355);
#1906=VERTEX_POINT('',#6357);
#1907=VERTEX_POINT('',#6361);
#1908=VERTEX_POINT('',#6363);
#1909=VERTEX_POINT('',#6367);
#1910=VERTEX_POINT('',#6369);
#1911=VERTEX_POINT('',#6373);
#1912=VERTEX_POINT('',#6375);
#1913=VERTEX_POINT('',#6379);
#1914=VERTEX_POINT('',#6381);
#1915=VERTEX_POINT('',#6385);
#1916=VERTEX_POINT('',#6387);
#1917=VERTEX_POINT('',#6391);
#1918=VERTEX_POINT('',#6392);
#1919=VERTEX_POINT('',#6394);
#1920=VERTEX_POINT('',#6396);
#1921=VERTEX_POINT('',#6400);
#1922=VERTEX_POINT('',#6402);
#1923=VERTEX_POINT('',#6406);
#1924=VERTEX_POINT('',#6408);
#1925=VERTEX_POINT('',#6412);
#1926=VERTEX_POINT('',#6414);
#1927=VERTEX_POINT('',#6418);
#1928=VERTEX_POINT('',#6420);
#1929=VERTEX_POINT('',#6424);
#1930=VERTEX_POINT('',#6426);
#1931=VERTEX_POINT('',#6430);
#1932=VERTEX_POINT('',#6432);
#1933=VERTEX_POINT('',#6436);
#1934=VERTEX_POINT('',#6438);
#1935=VERTEX_POINT('',#6442);
#1936=VERTEX_POINT('',#6444);
#1937=VERTEX_POINT('',#6448);
#1938=VERTEX_POINT('',#6450);
#1939=VERTEX_POINT('',#6454);
#1940=VERTEX_POINT('',#6456);
#1941=VERTEX_POINT('',#6460);
#1942=VERTEX_POINT('',#6462);
#1943=VERTEX_POINT('',#6469);
#1944=VERTEX_POINT('',#6471);
#1945=VERTEX_POINT('',#6478);
#1946=VERTEX_POINT('',#6480);
#1947=VERTEX_POINT('',#6494);
#1948=VERTEX_POINT('',#6496);
#1949=VERTEX_POINT('',#6501);
#1950=VERTEX_POINT('',#6503);
#1951=VERTEX_POINT('',#6508);
#1952=VERTEX_POINT('',#6510);
#1953=VERTEX_POINT('',#6513);
#1954=VERTEX_POINT('',#6515);
#1955=VERTEX_POINT('',#6520);
#1956=VERTEX_POINT('',#6524);
#1957=VERTEX_POINT('',#6531);
#1958=VERTEX_POINT('',#6532);
#1959=VERTEX_POINT('',#6534);
#1960=VERTEX_POINT('',#6536);
#1961=VERTEX_POINT('',#6540);
#1962=VERTEX_POINT('',#6541);
#1963=VERTEX_POINT('',#6543);
#1964=VERTEX_POINT('',#6545);
#1965=VERTEX_POINT('',#6551);
#1966=VERTEX_POINT('',#6554);
#1967=VERTEX_POINT('',#6555);
#1968=VERTEX_POINT('',#6557);
#1969=VERTEX_POINT('',#6559);
#1970=VERTEX_POINT('',#6563);
#1971=VERTEX_POINT('',#6564);
#1972=VERTEX_POINT('',#6566);
#1973=VERTEX_POINT('',#6568);
#1974=VERTEX_POINT('',#6574);
#1975=VERTEX_POINT('',#6577);
#1976=VERTEX_POINT('',#6579);
#1977=VERTEX_POINT('',#6581);
#1978=VERTEX_POINT('',#6583);
#1979=VERTEX_POINT('',#6587);
#1980=VERTEX_POINT('',#6590);
#1981=VERTEX_POINT('',#6594);
#1982=VERTEX_POINT('',#6600);
#1983=VERTEX_POINT('',#6604);
#1984=VERTEX_POINT('',#6608);
#1985=VERTEX_POINT('',#6612);
#1986=VERTEX_POINT('',#6614);
#1987=VERTEX_POINT('',#6618);
#1988=VERTEX_POINT('',#6619);
#1989=VERTEX_POINT('',#6621);
#1990=VERTEX_POINT('',#6623);
#1991=VERTEX_POINT('',#6627);
#1992=VERTEX_POINT('',#6629);
#1993=VERTEX_POINT('',#6633);
#1994=VERTEX_POINT('',#6635);
#1995=VERTEX_POINT('',#6648);
#1996=VERTEX_POINT('',#6649);
#1997=VERTEX_POINT('',#6651);
#1998=VERTEX_POINT('',#6653);
#1999=VERTEX_POINT('',#6657);
#2000=VERTEX_POINT('',#6658);
#2001=VERTEX_POINT('',#6660);
#2002=VERTEX_POINT('',#6662);
#2003=VERTEX_POINT('',#6668);
#2004=VERTEX_POINT('',#6671);
#2005=VERTEX_POINT('',#6672);
#2006=VERTEX_POINT('',#6674);
#2007=VERTEX_POINT('',#6676);
#2008=VERTEX_POINT('',#6680);
#2009=VERTEX_POINT('',#6681);
#2010=VERTEX_POINT('',#6683);
#2011=VERTEX_POINT('',#6685);
#2012=VERTEX_POINT('',#6691);
#2013=VERTEX_POINT('',#6694);
#2014=VERTEX_POINT('',#6696);
#2015=VERTEX_POINT('',#6698);
#2016=VERTEX_POINT('',#6700);
#2017=VERTEX_POINT('',#6704);
#2018=VERTEX_POINT('',#6707);
#2019=VERTEX_POINT('',#6711);
#2020=VERTEX_POINT('',#6717);
#2021=VERTEX_POINT('',#6721);
#2022=VERTEX_POINT('',#6725);
#2023=VERTEX_POINT('',#6729);
#2024=VERTEX_POINT('',#6731);
#2025=VERTEX_POINT('',#6735);
#2026=VERTEX_POINT('',#6736);
#2027=VERTEX_POINT('',#6738);
#2028=VERTEX_POINT('',#6740);
#2029=VERTEX_POINT('',#6744);
#2030=VERTEX_POINT('',#6746);
#2031=VERTEX_POINT('',#6750);
#2032=VERTEX_POINT('',#6752);
#2033=VERTEX_POINT('',#6765);
#2034=VERTEX_POINT('',#6766);
#2035=VERTEX_POINT('',#6768);
#2036=VERTEX_POINT('',#6770);
#2037=VERTEX_POINT('',#6774);
#2038=VERTEX_POINT('',#6776);
#2039=VERTEX_POINT('',#6780);
#2040=VERTEX_POINT('',#6782);
#2041=VERTEX_POINT('',#6786);
#2042=VERTEX_POINT('',#6788);
#2043=VERTEX_POINT('',#6792);
#2044=VERTEX_POINT('',#6794);
#2045=VERTEX_POINT('',#6803);
#2046=VERTEX_POINT('',#6806);
#2047=VERTEX_POINT('',#6809);
#2048=VERTEX_POINT('',#6813);
#2049=VERTEX_POINT('',#6817);
#2050=VERTEX_POINT('',#6821);
#2051=VERTEX_POINT('',#6824);
#2052=VERTEX_POINT('',#6831);
#2053=VERTEX_POINT('',#6832);
#2054=VERTEX_POINT('',#6834);
#2055=VERTEX_POINT('',#6836);
#2056=VERTEX_POINT('',#6840);
#2057=VERTEX_POINT('',#6842);
#2058=VERTEX_POINT('',#6846);
#2059=VERTEX_POINT('',#6848);
#2060=VERTEX_POINT('',#6851);
#2061=VERTEX_POINT('',#6854);
#2062=VERTEX_POINT('',#6856);
#2063=VERTEX_POINT('',#6858);
#2064=VERTEX_POINT('',#6860);
#2065=VERTEX_POINT('',#6862);
#2066=VERTEX_POINT('',#6864);
#2067=VERTEX_POINT('',#6868);
#2068=VERTEX_POINT('',#6872);
#2069=VERTEX_POINT('',#6876);
#2070=VERTEX_POINT('',#6878);
#2071=VERTEX_POINT('',#6880);
#2072=VERTEX_POINT('',#6882);
#2073=VERTEX_POINT('',#6888);
#2074=VERTEX_POINT('',#6890);
#2075=VERTEX_POINT('',#6894);
#2076=VERTEX_POINT('',#6897);
#2077=VERTEX_POINT('',#6899);
#2078=VERTEX_POINT('',#6912);
#2079=VERTEX_POINT('',#6913);
#2080=VERTEX_POINT('',#6916);
#2081=VERTEX_POINT('',#6918);
#2082=VERTEX_POINT('',#6922);
#2083=VERTEX_POINT('',#6926);
#2084=VERTEX_POINT('',#6928);
#2085=VERTEX_POINT('',#6932);
#2086=VERTEX_POINT('',#6937);
#2087=VERTEX_POINT('',#6941);
#2088=VERTEX_POINT('',#6947);
#2089=VERTEX_POINT('',#6948);
#2090=VERTEX_POINT('',#6951);
#2091=VERTEX_POINT('',#6953);
#2092=VERTEX_POINT('',#6957);
#2093=VERTEX_POINT('',#6961);
#2094=VERTEX_POINT('',#6963);
#2095=VERTEX_POINT('',#6966);
#2096=VERTEX_POINT('',#6970);
#2097=VERTEX_POINT('',#6974);
#2098=VERTEX_POINT('',#6982);
#2099=VERTEX_POINT('',#6983);
#2100=VERTEX_POINT('',#6986);
#2101=VERTEX_POINT('',#6987);
#2102=VERTEX_POINT('',#6990);
#2103=VERTEX_POINT('',#6991);
#2104=VERTEX_POINT('',#6994);
#2105=VERTEX_POINT('',#6995);
#2106=VERTEX_POINT('',#6998);
#2107=VERTEX_POINT('',#6999);
#2108=VERTEX_POINT('',#7002);
#2109=VERTEX_POINT('',#7003);
#2110=VERTEX_POINT('',#7006);
#2111=VERTEX_POINT('',#7007);
#2112=VERTEX_POINT('',#7010);
#2113=VERTEX_POINT('',#7011);
#2114=VERTEX_POINT('',#7015);
#2115=VERTEX_POINT('',#7016);
#2116=VERTEX_POINT('',#7039);
#2117=VERTEX_POINT('',#7041);
#2118=VERTEX_POINT('',#7066);
#2119=VERTEX_POINT('',#7068);
#2120=VERTEX_POINT('',#7091);
#2121=VERTEX_POINT('',#7093);
#2122=VERTEX_POINT('',#7116);
#2123=VERTEX_POINT('',#7118);
#2124=VERTEX_POINT('',#7131);
#2125=VERTEX_POINT('',#7134);
#2126=VERTEX_POINT('',#7147);
#2127=VERTEX_POINT('',#7149);
#2128=VERTEX_POINT('',#7172);
#2129=VERTEX_POINT('',#7174);
#2130=VERTEX_POINT('',#7197);
#2131=VERTEX_POINT('',#7199);
#2132=VERTEX_POINT('',#7222);
#2133=VERTEX_POINT('',#7224);
#2134=VERTEX_POINT('',#7249);
#2135=VERTEX_POINT('',#7253);
#2136=VERTEX_POINT('',#7278);
#2137=VERTEX_POINT('',#7282);
#2138=VERTEX_POINT('',#7307);
#2139=VERTEX_POINT('',#7311);
#2140=VERTEX_POINT('',#7312);
#2141=VERTEX_POINT('',#7339);
#2142=VERTEX_POINT('',#7343);
#2143=VERTEX_POINT('',#7368);
#2144=VERTEX_POINT('',#7372);
#2145=VERTEX_POINT('',#7397);
#2146=VERTEX_POINT('',#7401);
#2147=VERTEX_POINT('',#7426);
#2148=VERTEX_POINT('',#7429);
#2149=VERTEX_POINT('',#7431);
#2150=VERTEX_POINT('',#7463);
#2151=VERTEX_POINT('',#7465);
#2152=VERTEX_POINT('',#7468);
#2153=VERTEX_POINT('',#7472);
#2154=VERTEX_POINT('',#7477);
#2155=VERTEX_POINT('',#7479);
#2156=VERTEX_POINT('',#7482);
#2157=VERTEX_POINT('',#7486);
#2158=VERTEX_POINT('',#7497);
#2159=VERTEX_POINT('',#7499);
#2160=VERTEX_POINT('',#7503);
#2161=VERTEX_POINT('',#7505);
#2162=VERTEX_POINT('',#7512);
#2163=VERTEX_POINT('',#7514);
#2164=VERTEX_POINT('',#7518);
#2165=VERTEX_POINT('',#7520);
#2166=VERTEX_POINT('',#7527);
#2167=VERTEX_POINT('',#7529);
#2168=VERTEX_POINT('',#7533);
#2169=VERTEX_POINT('',#7535);
#2170=VERTEX_POINT('',#7543);
#2171=VERTEX_POINT('',#7545);
#2172=VERTEX_POINT('',#7549);
#2173=VERTEX_POINT('',#7551);
#2174=VERTEX_POINT('',#7558);
#2175=VERTEX_POINT('',#7560);
#2176=VERTEX_POINT('',#7564);
#2177=VERTEX_POINT('',#7566);
#2178=VERTEX_POINT('',#7570);
#2179=VERTEX_POINT('',#7572);
#2180=VERTEX_POINT('',#7576);
#2181=VERTEX_POINT('',#7578);
#2182=VERTEX_POINT('',#7582);
#2183=VERTEX_POINT('',#7584);
#2184=VERTEX_POINT('',#7588);
#2185=VERTEX_POINT('',#7591);
#2186=VERTEX_POINT('',#7595);
#2187=VERTEX_POINT('',#7597);
#2188=VERTEX_POINT('',#7604);
#2189=VERTEX_POINT('',#7606);
#2190=VERTEX_POINT('',#7610);
#2191=VERTEX_POINT('',#7612);
#2192=VERTEX_POINT('',#7616);
#2193=VERTEX_POINT('',#7618);
#2194=VERTEX_POINT('',#7622);
#2195=VERTEX_POINT('',#7624);
#2196=VERTEX_POINT('',#7628);
#2197=VERTEX_POINT('',#7630);
#2198=VERTEX_POINT('',#7634);
#2199=VERTEX_POINT('',#7636);
#2200=VERTEX_POINT('',#7643);
#2201=VERTEX_POINT('',#7646);
#2202=VERTEX_POINT('',#7650);
#2203=VERTEX_POINT('',#7654);
#2204=VERTEX_POINT('',#7658);
#2205=VERTEX_POINT('',#7661);
#2206=VERTEX_POINT('',#7665);
#2207=VERTEX_POINT('',#7669);
#2208=VERTEX_POINT('',#7674);
#2209=VERTEX_POINT('',#7675);
#2210=VERTEX_POINT('',#7677);
#2211=VERTEX_POINT('',#7679);
#2212=VERTEX_POINT('',#7683);
#2213=VERTEX_POINT('',#7685);
#2214=VERTEX_POINT('',#7689);
#2215=VERTEX_POINT('',#7691);
#2216=VERTEX_POINT('',#7695);
#2217=VERTEX_POINT('',#7697);
#2218=VERTEX_POINT('',#7701);
#2219=VERTEX_POINT('',#7703);
#2220=EDGE_CURVE('',#1857,#1858,#1175,.T.);
#2221=EDGE_CURVE('',#1857,#1859,#1176,.T.);
#2222=EDGE_CURVE('',#1860,#1859,#1177,.T.);
#2223=EDGE_CURVE('',#1858,#1860,#1178,.T.);
#2224=EDGE_CURVE('',#1861,#1857,#1179,.T.);
#2225=EDGE_CURVE('',#1861,#1862,#1180,.T.);
#2226=EDGE_CURVE('',#1859,#1862,#1181,.T.);
#2227=EDGE_CURVE('',#1863,#1861,#1182,.T.);
#2228=EDGE_CURVE('',#1863,#1864,#1183,.T.);
#2229=EDGE_CURVE('',#1862,#1864,#1184,.T.);
#2230=EDGE_CURVE('',#1865,#1863,#1185,.T.);
#2231=EDGE_CURVE('',#1865,#1866,#1186,.T.);
#2232=EDGE_CURVE('',#1864,#1866,#1187,.T.);
#2233=EDGE_CURVE('',#1867,#1865,#1188,.T.);
#2234=EDGE_CURVE('',#1867,#1868,#1189,.T.);
#2235=EDGE_CURVE('',#1866,#1868,#1190,.T.);
#2236=EDGE_CURVE('',#1869,#1867,#1191,.T.);
#2237=EDGE_CURVE('',#1869,#1870,#1192,.T.);
#2238=EDGE_CURVE('',#1868,#1870,#1193,.T.);
#2239=EDGE_CURVE('',#1871,#1869,#1194,.T.);
#2240=EDGE_CURVE('',#1871,#1872,#1195,.T.);
#2241=EDGE_CURVE('',#1870,#1872,#1196,.T.);
#2242=EDGE_CURVE('',#1873,#1871,#1197,.T.);
#2243=EDGE_CURVE('',#1873,#1874,#1198,.T.);
#2244=EDGE_CURVE('',#1872,#1874,#1199,.T.);
#2245=EDGE_CURVE('',#1875,#1873,#1200,.T.);
#2246=EDGE_CURVE('',#1876,#1875,#1201,.T.);
#2247=EDGE_CURVE('',#1874,#1876,#1202,.T.);
#2248=EDGE_CURVE('',#1877,#1878,#1203,.T.);
#2249=EDGE_CURVE('',#1877,#1879,#1204,.T.);
#2250=EDGE_CURVE('',#1880,#1879,#1205,.T.);
#2251=EDGE_CURVE('',#1878,#1880,#1206,.T.);
#2252=EDGE_CURVE('',#1881,#1877,#1207,.T.);
#2253=EDGE_CURVE('',#1881,#1882,#1208,.T.);
#2254=EDGE_CURVE('',#1879,#1882,#1209,.T.);
#2255=EDGE_CURVE('',#1883,#1881,#1210,.T.);
#2256=EDGE_CURVE('',#1883,#1884,#1211,.T.);
#2257=EDGE_CURVE('',#1882,#1884,#1212,.T.);
#2258=EDGE_CURVE('',#1885,#1883,#1213,.T.);
#2259=EDGE_CURVE('',#1885,#1886,#1214,.T.);
#2260=EDGE_CURVE('',#1884,#1886,#1215,.T.);
#2261=EDGE_CURVE('',#1887,#1885,#1216,.T.);
#2262=EDGE_CURVE('',#1887,#1888,#1217,.T.);
#2263=EDGE_CURVE('',#1886,#1888,#1218,.T.);
#2264=EDGE_CURVE('',#1889,#1887,#1219,.T.);
#2265=EDGE_CURVE('',#1889,#1890,#1220,.T.);
#2266=EDGE_CURVE('',#1888,#1890,#1221,.T.);
#2267=EDGE_CURVE('',#1891,#1889,#1222,.T.);
#2268=EDGE_CURVE('',#1891,#1892,#1223,.T.);
#2269=EDGE_CURVE('',#1890,#1892,#1224,.T.);
#2270=EDGE_CURVE('',#1893,#1891,#1225,.T.);
#2271=EDGE_CURVE('',#1893,#1894,#1226,.T.);
#2272=EDGE_CURVE('',#1892,#1894,#1227,.T.);
#2273=EDGE_CURVE('',#1895,#1893,#1228,.T.);
#2274=EDGE_CURVE('',#1896,#1895,#1229,.T.);
#2275=EDGE_CURVE('',#1894,#1896,#1230,.T.);
#2276=EDGE_CURVE('',#1897,#1898,#1231,.T.);
#2277=EDGE_CURVE('',#1897,#1899,#1232,.T.);
#2278=EDGE_CURVE('',#1900,#1899,#1233,.T.);
#2279=EDGE_CURVE('',#1898,#1900,#1234,.T.);
#2280=EDGE_CURVE('',#1901,#1897,#1235,.T.);
#2281=EDGE_CURVE('',#1901,#1902,#1236,.T.);
#2282=EDGE_CURVE('',#1899,#1902,#1237,.T.);
#2283=EDGE_CURVE('',#1903,#1901,#1238,.T.);
#2284=EDGE_CURVE('',#1903,#1904,#1239,.T.);
#2285=EDGE_CURVE('',#1902,#1904,#1240,.T.);
#2286=EDGE_CURVE('',#1905,#1903,#1241,.T.);
#2287=EDGE_CURVE('',#1905,#1906,#1242,.T.);
#2288=EDGE_CURVE('',#1904,#1906,#1243,.T.);
#2289=EDGE_CURVE('',#1907,#1905,#1244,.T.);
#2290=EDGE_CURVE('',#1907,#1908,#1245,.T.);
#2291=EDGE_CURVE('',#1906,#1908,#1246,.T.);
#2292=EDGE_CURVE('',#1909,#1907,#1247,.T.);
#2293=EDGE_CURVE('',#1909,#1910,#1248,.T.);
#2294=EDGE_CURVE('',#1908,#1910,#1249,.T.);
#2295=EDGE_CURVE('',#1911,#1909,#1250,.T.);
#2296=EDGE_CURVE('',#1911,#1912,#1251,.T.);
#2297=EDGE_CURVE('',#1910,#1912,#1252,.T.);
#2298=EDGE_CURVE('',#1913,#1911,#1253,.T.);
#2299=EDGE_CURVE('',#1913,#1914,#1254,.T.);
#2300=EDGE_CURVE('',#1912,#1914,#1255,.T.);
#2301=EDGE_CURVE('',#1915,#1913,#1256,.T.);
#2302=EDGE_CURVE('',#1916,#1915,#1257,.T.);
#2303=EDGE_CURVE('',#1914,#1916,#1258,.T.);
#2304=EDGE_CURVE('',#1917,#1918,#1259,.T.);
#2305=EDGE_CURVE('',#1917,#1919,#1260,.T.);
#2306=EDGE_CURVE('',#1920,#1919,#1261,.T.);
#2307=EDGE_CURVE('',#1918,#1920,#1262,.T.);
#2308=EDGE_CURVE('',#1921,#1917,#1263,.T.);
#2309=EDGE_CURVE('',#1921,#1922,#1264,.T.);
#2310=EDGE_CURVE('',#1919,#1922,#1265,.T.);
#2311=EDGE_CURVE('',#1923,#1921,#1266,.T.);
#2312=EDGE_CURVE('',#1923,#1924,#1267,.T.);
#2313=EDGE_CURVE('',#1922,#1924,#1268,.T.);
#2314=EDGE_CURVE('',#1925,#1923,#1269,.T.);
#2315=EDGE_CURVE('',#1925,#1926,#1270,.T.);
#2316=EDGE_CURVE('',#1924,#1926,#1271,.T.);
#2317=EDGE_CURVE('',#1927,#1925,#1272,.T.);
#2318=EDGE_CURVE('',#1927,#1928,#1273,.T.);
#2319=EDGE_CURVE('',#1926,#1928,#1274,.T.);
#2320=EDGE_CURVE('',#1929,#1927,#1275,.T.);
#2321=EDGE_CURVE('',#1929,#1930,#1276,.T.);
#2322=EDGE_CURVE('',#1928,#1930,#1277,.T.);
#2323=EDGE_CURVE('',#1931,#1929,#1278,.T.);
#2324=EDGE_CURVE('',#1931,#1932,#1279,.T.);
#2325=EDGE_CURVE('',#1930,#1932,#1280,.T.);
#2326=EDGE_CURVE('',#1933,#1931,#1281,.T.);
#2327=EDGE_CURVE('',#1933,#1934,#1282,.T.);
#2328=EDGE_CURVE('',#1932,#1934,#1283,.T.);
#2329=EDGE_CURVE('',#1935,#1933,#1284,.T.);
#2330=EDGE_CURVE('',#1936,#1935,#1285,.T.);
#2331=EDGE_CURVE('',#1934,#1936,#1286,.T.);
#2332=EDGE_CURVE('',#1937,#1937,#421,.T.);
#2333=EDGE_CURVE('',#1937,#1938,#1287,.T.);
#2334=EDGE_CURVE('',#1938,#1938,#422,.T.);
#2335=EDGE_CURVE('',#1875,#1939,#1288,.T.);
#2336=EDGE_CURVE('',#1939,#1940,#1289,.T.);
#2337=EDGE_CURVE('',#1876,#1940,#1290,.T.);
#2338=EDGE_CURVE('',#1941,#1860,#1291,.T.);
#2339=EDGE_CURVE('',#1942,#1941,#1292,.T.);
#2340=EDGE_CURVE('',#1942,#1858,#1293,.T.);
#2341=EDGE_CURVE('',#1895,#1942,#1294,.T.);
#2342=EDGE_CURVE('',#1896,#1941,#1295,.T.);
#2343=EDGE_CURVE('',#1943,#1880,#1296,.T.);
#2344=EDGE_CURVE('',#1944,#1943,#1297,.T.);
#2345=EDGE_CURVE('',#1944,#1878,#1298,.T.);
#2346=EDGE_CURVE('',#1915,#1944,#1299,.T.);
#2347=EDGE_CURVE('',#1916,#1943,#1300,.T.);
#2348=EDGE_CURVE('',#1945,#1900,#1301,.T.);
#2349=EDGE_CURVE('',#1946,#1945,#1302,.T.);
#2350=EDGE_CURVE('',#1946,#1898,#1303,.T.);
#2351=EDGE_CURVE('',#1935,#1946,#1304,.T.);
#2352=EDGE_CURVE('',#1936,#1945,#1305,.T.);
#2353=EDGE_CURVE('',#1940,#1920,#1306,.T.);
#2354=EDGE_CURVE('',#1939,#1918,#1307,.T.);
#2355=EDGE_CURVE('',#1947,#1947,#423,.T.);
#2356=EDGE_CURVE('',#1947,#1948,#1308,.T.);
#2357=EDGE_CURVE('',#1948,#1948,#424,.T.);
#2358=EDGE_CURVE('',#1949,#1949,#425,.T.);
#2359=EDGE_CURVE('',#1949,#1950,#1309,.T.);
#2360=EDGE_CURVE('',#1950,#1950,#426,.T.);
#2361=EDGE_CURVE('',#1951,#1951,#427,.T.);
#2362=EDGE_CURVE('',#1952,#1952,#428,.T.);
#2363=EDGE_CURVE('',#1953,#1953,#429,.T.);
#2364=EDGE_CURVE('',#1954,#1954,#430,.T.);
#2365=EDGE_CURVE('',#1951,#1953,#1310,.T.);
#2366=EDGE_CURVE('',#1954,#1955,#1311,.T.);
#2367=EDGE_CURVE('',#1955,#1955,#431,.T.);
#2368=EDGE_CURVE('',#1956,#1956,#432,.T.);
#2369=EDGE_CURVE('',#1956,#1952,#1312,.T.);
#2370=EDGE_CURVE('',#1957,#1958,#1313,.T.);
#2371=EDGE_CURVE('',#1959,#1957,#433,.T.);
#2372=EDGE_CURVE('',#1960,#1959,#1314,.T.);
#2373=EDGE_CURVE('',#1958,#1960,#434,.T.);
#2374=EDGE_CURVE('',#1961,#1962,#1315,.T.);
#2375=EDGE_CURVE('',#1963,#1961,#435,.T.);
#2376=EDGE_CURVE('',#1964,#1963,#1316,.T.);
#2377=EDGE_CURVE('',#1962,#1964,#436,.T.);
#2378=EDGE_CURVE('',#1958,#1961,#1317,.T.);
#2379=EDGE_CURVE('',#1963,#1960,#1318,.T.);
#2380=EDGE_CURVE('',#1965,#1965,#437,.T.);
#2381=EDGE_CURVE('',#1966,#1967,#1319,.T.);
#2382=EDGE_CURVE('',#1968,#1966,#438,.T.);
#2383=EDGE_CURVE('',#1969,#1968,#1320,.T.);
#2384=EDGE_CURVE('',#1967,#1969,#439,.T.);
#2385=EDGE_CURVE('',#1970,#1971,#1321,.T.);
#2386=EDGE_CURVE('',#1972,#1970,#440,.T.);
#2387=EDGE_CURVE('',#1973,#1972,#1322,.T.);
#2388=EDGE_CURVE('',#1971,#1973,#441,.T.);
#2389=EDGE_CURVE('',#1967,#1970,#1323,.T.);
#2390=EDGE_CURVE('',#1972,#1969,#1324,.T.);
#2391=EDGE_CURVE('',#1974,#1974,#442,.T.);
#2392=EDGE_CURVE('',#1975,#1959,#1325,.T.);
#2393=EDGE_CURVE('',#1976,#1975,#1326,.T.);
#2394=EDGE_CURVE('',#1976,#1977,#1327,.T.);
#2395=EDGE_CURVE('',#1977,#1978,#1328,.T.);
#2396=EDGE_CURVE('',#1973,#1978,#1329,.T.);
#2397=EDGE_CURVE('',#1964,#1968,#1330,.T.);
#2398=EDGE_CURVE('',#1979,#1979,#443,.T.);
#2399=EDGE_CURVE('',#1978,#1980,#1331,.T.);
#2400=EDGE_CURVE('',#1980,#1971,#1332,.T.);
#2401=EDGE_CURVE('',#1957,#1981,#1333,.T.);
#2402=EDGE_CURVE('',#1981,#1975,#1334,.T.);
#2403=EDGE_CURVE('',#1966,#1962,#1335,.T.);
#2404=EDGE_CURVE('',#1982,#1982,#444,.T.);
#2405=EDGE_CURVE('',#1982,#1965,#1336,.T.);
#2406=EDGE_CURVE('',#1983,#1983,#445,.T.);
#2407=EDGE_CURVE('',#1983,#1974,#1337,.T.);
#2408=EDGE_CURVE('',#1979,#1984,#1338,.T.);
#2409=EDGE_CURVE('',#1984,#1984,#446,.T.);
#2410=EDGE_CURVE('',#1985,#1976,#1339,.T.);
#2411=EDGE_CURVE('',#1986,#1985,#1340,.T.);
#2412=EDGE_CURVE('',#1986,#1977,#1341,.T.);
#2413=EDGE_CURVE('',#1987,#1988,#1342,.T.);
#2414=EDGE_CURVE('',#1987,#1989,#1343,.T.);
#2415=EDGE_CURVE('',#1990,#1989,#1344,.T.);
#2416=EDGE_CURVE('',#1988,#1990,#1345,.T.);
#2417=EDGE_CURVE('',#1989,#1991,#1346,.T.);
#2418=EDGE_CURVE('',#1991,#1992,#1347,.T.);
#2419=EDGE_CURVE('',#1992,#1990,#1348,.T.);
#2420=EDGE_CURVE('',#1985,#1993,#1349,.T.);
#2421=EDGE_CURVE('',#1993,#1994,#1350,.T.);
#2422=EDGE_CURVE('',#1994,#1986,#1351,.T.);
#2423=EDGE_CURVE('',#1987,#1980,#1352,.T.);
#2424=EDGE_CURVE('',#1988,#1981,#1353,.T.);
#2425=EDGE_CURVE('',#1992,#1993,#1354,.T.);
#2426=EDGE_CURVE('',#1994,#1991,#1355,.T.);
#2427=EDGE_CURVE('',#1995,#1996,#1356,.T.);
#2428=EDGE_CURVE('',#1997,#1995,#447,.T.);
#2429=EDGE_CURVE('',#1998,#1997,#1357,.T.);
#2430=EDGE_CURVE('',#1996,#1998,#448,.T.);
#2431=EDGE_CURVE('',#1999,#2000,#1358,.T.);
#2432=EDGE_CURVE('',#2001,#1999,#449,.T.);
#2433=EDGE_CURVE('',#2002,#2001,#1359,.T.);
#2434=EDGE_CURVE('',#2000,#2002,#450,.T.);
#2435=EDGE_CURVE('',#1996,#1999,#1360,.T.);
#2436=EDGE_CURVE('',#2001,#1998,#1361,.T.);
#2437=EDGE_CURVE('',#2003,#2003,#451,.T.);
#2438=EDGE_CURVE('',#2004,#2005,#1362,.T.);
#2439=EDGE_CURVE('',#2006,#2004,#452,.T.);
#2440=EDGE_CURVE('',#2007,#2006,#1363,.T.);
#2441=EDGE_CURVE('',#2005,#2007,#453,.T.);
#2442=EDGE_CURVE('',#2008,#2009,#1364,.T.);
#2443=EDGE_CURVE('',#2010,#2008,#454,.T.);
#2444=EDGE_CURVE('',#2011,#2010,#1365,.T.);
#2445=EDGE_CURVE('',#2009,#2011,#455,.T.);
#2446=EDGE_CURVE('',#2005,#2008,#1366,.T.);
#2447=EDGE_CURVE('',#2010,#2007,#1367,.T.);
#2448=EDGE_CURVE('',#2012,#2012,#456,.T.);
#2449=EDGE_CURVE('',#2013,#1997,#1368,.T.);
#2450=EDGE_CURVE('',#2014,#2013,#1369,.T.);
#2451=EDGE_CURVE('',#2014,#2015,#1370,.T.);
#2452=EDGE_CURVE('',#2015,#2016,#1371,.T.);
#2453=EDGE_CURVE('',#2011,#2016,#1372,.T.);
#2454=EDGE_CURVE('',#2002,#2006,#1373,.T.);
#2455=EDGE_CURVE('',#2017,#2017,#457,.T.);
#2456=EDGE_CURVE('',#2016,#2018,#1374,.T.);
#2457=EDGE_CURVE('',#2018,#2009,#1375,.T.);
#2458=EDGE_CURVE('',#1995,#2019,#1376,.T.);
#2459=EDGE_CURVE('',#2019,#2013,#1377,.T.);
#2460=EDGE_CURVE('',#2004,#2000,#1378,.T.);
#2461=EDGE_CURVE('',#2020,#2020,#458,.T.);
#2462=EDGE_CURVE('',#2020,#2003,#1379,.T.);
#2463=EDGE_CURVE('',#2021,#2021,#459,.T.);
#2464=EDGE_CURVE('',#2021,#2012,#1380,.T.);
#2465=EDGE_CURVE('',#2017,#2022,#1381,.T.);
#2466=EDGE_CURVE('',#2022,#2022,#460,.T.);
#2467=EDGE_CURVE('',#2023,#2014,#1382,.T.);
#2468=EDGE_CURVE('',#2024,#2023,#1383,.T.);
#2469=EDGE_CURVE('',#2024,#2015,#1384,.T.);
#2470=EDGE_CURVE('',#2025,#2026,#1385,.T.);
#2471=EDGE_CURVE('',#2025,#2027,#1386,.T.);
#2472=EDGE_CURVE('',#2028,#2027,#1387,.T.);
#2473=EDGE_CURVE('',#2026,#2028,#1388,.T.);
#2474=EDGE_CURVE('',#2027,#2029,#1389,.T.);
#2475=EDGE_CURVE('',#2029,#2030,#1390,.T.);
#2476=EDGE_CURVE('',#2030,#2028,#1391,.T.);
#2477=EDGE_CURVE('',#2023,#2031,#1392,.T.);
#2478=EDGE_CURVE('',#2031,#2032,#1393,.T.);
#2479=EDGE_CURVE('',#2032,#2024,#1394,.T.);
#2480=EDGE_CURVE('',#2025,#2018,#1395,.T.);
#2481=EDGE_CURVE('',#2026,#2019,#1396,.T.);
#2482=EDGE_CURVE('',#2030,#2031,#1397,.T.);
#2483=EDGE_CURVE('',#2032,#2029,#1398,.T.);
#2484=EDGE_CURVE('',#2033,#2034,#1399,.T.);
#2485=EDGE_CURVE('',#2034,#2035,#1400,.T.);
#2486=EDGE_CURVE('',#2035,#2036,#1401,.T.);
#2487=EDGE_CURVE('',#2033,#2036,#1402,.T.);
#2488=EDGE_CURVE('',#2034,#2037,#1403,.T.);
#2489=EDGE_CURVE('',#2037,#2038,#1404,.T.);
#2490=EDGE_CURVE('',#2038,#2035,#1405,.T.);
#2491=EDGE_CURVE('',#2037,#2039,#1406,.T.);
#2492=EDGE_CURVE('',#2039,#2040,#1407,.T.);
#2493=EDGE_CURVE('',#2040,#2038,#1408,.T.);
#2494=EDGE_CURVE('',#2039,#2041,#1409,.T.);
#2495=EDGE_CURVE('',#2041,#2042,#1410,.T.);
#2496=EDGE_CURVE('',#2042,#2040,#1411,.T.);
#2497=EDGE_CURVE('',#2041,#2043,#1412,.T.);
#2498=EDGE_CURVE('',#2043,#2044,#1413,.T.);
#2499=EDGE_CURVE('',#2044,#2042,#1414,.T.);
#2500=EDGE_CURVE('',#2043,#2033,#1415,.T.);
#2501=EDGE_CURVE('',#2036,#2044,#1416,.T.);
#2502=EDGE_CURVE('',#2045,#2045,#461,.T.);
#2503=EDGE_CURVE('',#2046,#2046,#462,.T.);
#2504=EDGE_CURVE('',#2047,#2047,#463,.T.);
#2505=EDGE_CURVE('',#2047,#2046,#1417,.T.);
#2506=EDGE_CURVE('',#2048,#2048,#464,.T.);
#2507=EDGE_CURVE('',#2048,#2047,#1418,.T.);
#2508=EDGE_CURVE('',#2049,#2049,#465,.T.);
#2509=EDGE_CURVE('',#2049,#2048,#1419,.T.);
#2510=EDGE_CURVE('',#2050,#2050,#466,.T.);
#2511=EDGE_CURVE('',#2051,#2051,#467,.F.);
#2512=EDGE_CURVE('',#2051,#2050,#1420,.T.);
#2513=EDGE_CURVE('',#2045,#2051,#1421,.T.);
#2514=EDGE_CURVE('',#2052,#2053,#1422,.T.);
#2515=EDGE_CURVE('',#2054,#2052,#1423,.T.);
#2516=EDGE_CURVE('',#2055,#2054,#1424,.T.);
#2517=EDGE_CURVE('',#2053,#2055,#1425,.T.);
#2518=EDGE_CURVE('',#2054,#2056,#1426,.T.);
#2519=EDGE_CURVE('',#2057,#2056,#1427,.T.);
#2520=EDGE_CURVE('',#2055,#2057,#1428,.T.);
#2521=EDGE_CURVE('',#2056,#2058,#1429,.T.);
#2522=EDGE_CURVE('',#2058,#2059,#1430,.T.);
#2523=EDGE_CURVE('',#2059,#2057,#1431,.T.);
#2524=EDGE_CURVE('',#2060,#2060,#468,.T.);
#2525=EDGE_CURVE('',#2061,#2052,#1432,.T.);
#2526=EDGE_CURVE('',#2062,#2061,#1433,.T.);
#2527=EDGE_CURVE('',#2062,#2063,#1434,.T.);
#2528=EDGE_CURVE('',#2064,#2063,#1435,.T.);
#2529=EDGE_CURVE('',#2064,#2065,#1436,.T.);
#2530=EDGE_CURVE('',#2065,#2066,#1437,.T.);
#2531=EDGE_CURVE('',#2066,#2058,#1438,.T.);
#2532=EDGE_CURVE('',#2066,#2067,#1439,.T.);
#2533=EDGE_CURVE('',#2067,#2059,#1440,.T.);
#2534=EDGE_CURVE('',#2068,#2065,#1441,.T.);
#2535=EDGE_CURVE('',#2067,#2068,#1442,.T.);
#2536=EDGE_CURVE('',#2069,#2068,#1443,.T.);
#2537=EDGE_CURVE('',#2070,#2069,#1444,.T.);
#2538=EDGE_CURVE('',#2070,#2071,#1445,.T.);
#2539=EDGE_CURVE('',#2072,#2071,#1446,.T.);
#2540=EDGE_CURVE('',#2072,#2053,#1447,.T.);
#2541=EDGE_CURVE('',#2069,#2064,#1448,.T.);
#2542=EDGE_CURVE('',#2063,#2073,#1449,.T.);
#2543=EDGE_CURVE('',#2073,#2074,#259,.T.);
#2544=EDGE_CURVE('',#2074,#2070,#1450,.T.);
#2545=EDGE_CURVE('',#2075,#2073,#469,.F.);
#2546=EDGE_CURVE('',#2075,#2060,#1451,.T.);
#2547=EDGE_CURVE('',#2076,#2075,#470,.F.);
#2548=EDGE_CURVE('',#2077,#2076,#260,.T.);
#2549=EDGE_CURVE('',#2074,#2077,#471,.F.);
#2550=EDGE_CURVE('',#2076,#2062,#1452,.T.);
#2551=EDGE_CURVE('',#2071,#2077,#1453,.T.);
#2552=EDGE_CURVE('',#2061,#2072,#1454,.T.);
#2553=EDGE_CURVE('',#2078,#2079,#472,.T.);
#2554=EDGE_CURVE('',#2079,#2078,#473,.T.);
#2555=EDGE_CURVE('',#2079,#2080,#474,.T.);
#2556=EDGE_CURVE('',#2081,#2080,#475,.T.);
#2557=EDGE_CURVE('',#2080,#2081,#476,.T.);
#2558=EDGE_CURVE('',#2081,#2082,#1455,.T.);
#2559=EDGE_CURVE('',#2082,#2082,#477,.T.);
#2560=EDGE_CURVE('',#2083,#2083,#478,.T.);
#2561=EDGE_CURVE('',#2083,#2084,#1456,.T.);
#2562=EDGE_CURVE('',#2084,#2084,#479,.T.);
#2563=EDGE_CURVE('',#2084,#2085,#1457,.T.);
#2564=EDGE_CURVE('',#2085,#2085,#480,.T.);
#2565=EDGE_CURVE('',#2086,#2086,#481,.T.);
#2566=EDGE_CURVE('',#2086,#2078,#1458,.T.);
#2567=EDGE_CURVE('',#2087,#2087,#482,.T.);
#2568=EDGE_CURVE('',#2087,#2083,#1459,.T.);
#2569=EDGE_CURVE('',#2088,#2089,#483,.T.);
#2570=EDGE_CURVE('',#2089,#2088,#484,.T.);
#2571=EDGE_CURVE('',#2089,#2090,#485,.T.);
#2572=EDGE_CURVE('',#2091,#2090,#486,.T.);
#2573=EDGE_CURVE('',#2090,#2091,#487,.T.);
#2574=EDGE_CURVE('',#2092,#2092,#488,.T.);
#2575=EDGE_CURVE('',#2092,#2091,#1460,.T.);
#2576=EDGE_CURVE('',#2093,#2093,#489,.T.);
#2577=EDGE_CURVE('',#2094,#2094,#490,.T.);
#2578=EDGE_CURVE('',#2095,#2095,#491,.T.);
#2579=EDGE_CURVE('',#2095,#2093,#1461,.T.);
#2580=EDGE_CURVE('',#2096,#2096,#492,.T.);
#2581=EDGE_CURVE('',#2096,#2095,#1462,.T.);
#2582=EDGE_CURVE('',#2097,#2097,#493,.T.);
#2583=EDGE_CURVE('',#2097,#2096,#1463,.T.);
#2584=EDGE_CURVE('',#2088,#2094,#1464,.T.);
#2585=EDGE_CURVE('',#2098,#2099,#494,.T.);
#2586=EDGE_CURVE('',#2100,#2101,#495,.T.);
#2587=EDGE_CURVE('',#2102,#2103,#496,.T.);
#2588=EDGE_CURVE('',#2104,#2105,#497,.T.);
#2589=EDGE_CURVE('',#2106,#2107,#498,.T.);
#2590=EDGE_CURVE('',#2108,#2109,#499,.T.);
#2591=EDGE_CURVE('',#2110,#2111,#500,.T.);
#2592=EDGE_CURVE('',#2112,#2113,#501,.T.);
#2593=EDGE_CURVE('',#2114,#2115,#223,.T.);
#2594=EDGE_CURVE('',#2116,#2114,#502,.T.);
#2595=EDGE_CURVE('',#2117,#2116,#224,.T.);
#2596=EDGE_CURVE('',#2115,#2117,#503,.T.);
#2597=EDGE_CURVE('',#2118,#2116,#504,.T.);
#2598=EDGE_CURVE('',#2118,#2119,#225,.T.);
#2599=EDGE_CURVE('',#2120,#2119,#505,.T.);
#2600=EDGE_CURVE('',#2120,#2121,#226,.T.);
#2601=EDGE_CURVE('',#2122,#2121,#506,.T.);
#2602=EDGE_CURVE('',#2122,#2123,#227,.T.);
#2603=EDGE_CURVE('',#2123,#2124,#1465,.T.);
#2604=EDGE_CURVE('',#2124,#2124,#507,.T.);
#2605=EDGE_CURVE('',#2123,#2125,#228,.T.);
#2606=EDGE_CURVE('',#2126,#2125,#508,.T.);
#2607=EDGE_CURVE('',#2126,#2127,#229,.T.);
#2608=EDGE_CURVE('',#2128,#2127,#509,.T.);
#2609=EDGE_CURVE('',#2128,#2129,#230,.T.);
#2610=EDGE_CURVE('',#2130,#2129,#510,.T.);
#2611=EDGE_CURVE('',#2130,#2131,#231,.T.);
#2612=EDGE_CURVE('',#2132,#2131,#511,.T.);
#2613=EDGE_CURVE('',#2132,#2133,#232,.T.);
#2614=EDGE_CURVE('',#2117,#2133,#512,.T.);
#2615=EDGE_CURVE('',#2114,#2134,#513,.T.);
#2616=EDGE_CURVE('',#2134,#2118,#514,.T.);
#2617=EDGE_CURVE('',#2135,#2134,#233,.T.);
#2618=EDGE_CURVE('',#2119,#2135,#515,.T.);
#2619=EDGE_CURVE('',#2135,#2136,#516,.T.);
#2620=EDGE_CURVE('',#2136,#2120,#517,.T.);
#2621=EDGE_CURVE('',#2137,#2136,#234,.T.);
#2622=EDGE_CURVE('',#2121,#2137,#518,.T.);
#2623=EDGE_CURVE('',#2137,#2138,#519,.T.);
#2624=EDGE_CURVE('',#2138,#2122,#520,.T.);
#2625=EDGE_CURVE('',#2139,#2140,#235,.T.);
#2626=EDGE_CURVE('',#2125,#2139,#521,.T.);
#2627=EDGE_CURVE('',#2140,#2138,#236,.T.);
#2628=EDGE_CURVE('',#2139,#2141,#522,.T.);
#2629=EDGE_CURVE('',#2141,#2126,#523,.T.);
#2630=EDGE_CURVE('',#2142,#2141,#237,.T.);
#2631=EDGE_CURVE('',#2127,#2142,#524,.T.);
#2632=EDGE_CURVE('',#2142,#2143,#525,.T.);
#2633=EDGE_CURVE('',#2143,#2128,#526,.T.);
#2634=EDGE_CURVE('',#2144,#2143,#238,.T.);
#2635=EDGE_CURVE('',#2129,#2144,#527,.T.);
#2636=EDGE_CURVE('',#2144,#2145,#528,.T.);
#2637=EDGE_CURVE('',#2145,#2130,#529,.T.);
#2638=EDGE_CURVE('',#2146,#2145,#239,.T.);
#2639=EDGE_CURVE('',#2131,#2146,#530,.T.);
#2640=EDGE_CURVE('',#2147,#2147,#531,.T.);
#2641=EDGE_CURVE('',#2147,#2140,#1466,.T.);
#2642=EDGE_CURVE('',#2148,#2115,#532,.T.);
#2643=EDGE_CURVE('',#2148,#2149,#240,.T.);
#2644=EDGE_CURVE('',#2146,#2149,#533,.T.);
#2645=EDGE_CURVE('',#2133,#2148,#534,.T.);
#2646=EDGE_CURVE('',#2149,#2132,#535,.T.);
#2647=EDGE_CURVE('',#2150,#2150,#536,.T.);
#2648=EDGE_CURVE('',#2151,#2151,#537,.T.);
#2649=EDGE_CURVE('',#2152,#2152,#538,.T.);
#2650=EDGE_CURVE('',#2152,#2150,#1467,.T.);
#2651=EDGE_CURVE('',#2153,#2153,#539,.T.);
#2652=EDGE_CURVE('',#2153,#2151,#1468,.T.);
#2653=EDGE_CURVE('',#2154,#2154,#540,.T.);
#2654=EDGE_CURVE('',#2155,#2155,#541,.T.);
#2655=EDGE_CURVE('',#2156,#2156,#542,.T.);
#2656=EDGE_CURVE('',#2156,#2154,#1469,.T.);
#2657=EDGE_CURVE('',#2157,#2157,#543,.T.);
#2658=EDGE_CURVE('',#2157,#2155,#1470,.T.);
#2659=EDGE_CURVE('',#2158,#2158,#544,.T.);
#2660=EDGE_CURVE('',#2158,#2159,#1471,.T.);
#2661=EDGE_CURVE('',#2159,#2159,#545,.T.);
#2662=EDGE_CURVE('',#2160,#2160,#546,.T.);
#2663=EDGE_CURVE('',#2160,#2161,#1472,.T.);
#2664=EDGE_CURVE('',#2161,#2161,#547,.T.);
#2665=EDGE_CURVE('',#2162,#2162,#548,.T.);
#2666=EDGE_CURVE('',#2162,#2163,#1473,.T.);
#2667=EDGE_CURVE('',#2163,#2163,#549,.T.);
#2668=EDGE_CURVE('',#2164,#2164,#550,.T.);
#2669=EDGE_CURVE('',#2164,#2165,#1474,.T.);
#2670=EDGE_CURVE('',#2165,#2165,#551,.T.);
#2671=EDGE_CURVE('',#2166,#2166,#552,.T.);
#2672=EDGE_CURVE('',#2166,#2167,#1475,.T.);
#2673=EDGE_CURVE('',#2167,#2167,#553,.T.);
#2674=EDGE_CURVE('',#2168,#2168,#554,.T.);
#2675=EDGE_CURVE('',#2168,#2169,#1476,.T.);
#2676=EDGE_CURVE('',#2169,#2169,#555,.T.);
#2677=EDGE_CURVE('',#2170,#2170,#556,.T.);
#2678=EDGE_CURVE('',#2170,#2171,#1477,.T.);
#2679=EDGE_CURVE('',#2171,#2171,#557,.T.);
#2680=EDGE_CURVE('',#2172,#2172,#558,.T.);
#2681=EDGE_CURVE('',#2172,#2173,#1478,.T.);
#2682=EDGE_CURVE('',#2173,#2173,#559,.T.);
#2683=EDGE_CURVE('',#2174,#2174,#560,.T.);
#2684=EDGE_CURVE('',#2174,#2175,#1479,.T.);
#2685=EDGE_CURVE('',#2175,#2175,#561,.T.);
#2686=EDGE_CURVE('',#2176,#2176,#562,.T.);
#2687=EDGE_CURVE('',#2176,#2177,#1480,.T.);
#2688=EDGE_CURVE('',#2177,#2177,#563,.T.);
#2689=EDGE_CURVE('',#2178,#2178,#564,.T.);
#2690=EDGE_CURVE('',#2178,#2179,#1481,.T.);
#2691=EDGE_CURVE('',#2179,#2179,#565,.T.);
#2692=EDGE_CURVE('',#2180,#2180,#566,.T.);
#2693=EDGE_CURVE('',#2180,#2181,#1482,.T.);
#2694=EDGE_CURVE('',#2181,#2181,#567,.T.);
#2695=EDGE_CURVE('',#2182,#2182,#568,.T.);
#2696=EDGE_CURVE('',#2182,#2183,#1483,.T.);
#2697=EDGE_CURVE('',#2183,#2183,#569,.T.);
#2698=EDGE_CURVE('',#2184,#2184,#570,.T.);
#2699=EDGE_CURVE('',#2184,#2185,#1484,.T.);
#2700=EDGE_CURVE('',#2185,#2185,#571,.T.);
#2701=EDGE_CURVE('',#2186,#2186,#572,.T.);
#2702=EDGE_CURVE('',#2186,#2187,#1485,.T.);
#2703=EDGE_CURVE('',#2187,#2187,#573,.T.);
#2704=EDGE_CURVE('',#2188,#2188,#574,.T.);
#2705=EDGE_CURVE('',#2188,#2189,#1486,.T.);
#2706=EDGE_CURVE('',#2189,#2189,#575,.T.);
#2707=EDGE_CURVE('',#2190,#2190,#576,.T.);
#2708=EDGE_CURVE('',#2190,#2191,#1487,.T.);
#2709=EDGE_CURVE('',#2191,#2191,#577,.T.);
#2710=EDGE_CURVE('',#2192,#2192,#578,.T.);
#2711=EDGE_CURVE('',#2192,#2193,#1488,.T.);
#2712=EDGE_CURVE('',#2193,#2193,#579,.T.);
#2713=EDGE_CURVE('',#2194,#2194,#580,.T.);
#2714=EDGE_CURVE('',#2194,#2195,#1489,.T.);
#2715=EDGE_CURVE('',#2195,#2195,#581,.T.);
#2716=EDGE_CURVE('',#2196,#2196,#582,.T.);
#2717=EDGE_CURVE('',#2196,#2197,#1490,.T.);
#2718=EDGE_CURVE('',#2197,#2197,#583,.T.);
#2719=EDGE_CURVE('',#2198,#2198,#584,.T.);
#2720=EDGE_CURVE('',#2198,#2199,#1491,.T.);
#2721=EDGE_CURVE('',#2199,#2199,#585,.T.);
#2722=EDGE_CURVE('',#2200,#2200,#586,.T.);
#2723=EDGE_CURVE('',#2201,#2201,#587,.T.);
#2724=EDGE_CURVE('',#2201,#2200,#1492,.T.);
#2725=EDGE_CURVE('',#2202,#2202,#588,.T.);
#2726=EDGE_CURVE('',#2202,#2201,#1493,.T.);
#2727=EDGE_CURVE('',#2203,#2203,#589,.T.);
#2728=EDGE_CURVE('',#2203,#2202,#1494,.T.);
#2729=EDGE_CURVE('',#2204,#2204,#590,.T.);
#2730=EDGE_CURVE('',#2205,#2205,#591,.F.);
#2731=EDGE_CURVE('',#2205,#2204,#1495,.T.);
#2732=EDGE_CURVE('',#2206,#2206,#592,.F.);
#2733=EDGE_CURVE('',#2206,#2205,#1496,.T.);
#2734=EDGE_CURVE('',#2207,#2207,#593,.T.);
#2735=EDGE_CURVE('',#2207,#2206,#1497,.T.);
#2736=EDGE_CURVE('',#2208,#2209,#1498,.T.);
#2737=EDGE_CURVE('',#2209,#2210,#1499,.T.);
#2738=EDGE_CURVE('',#2210,#2211,#1500,.T.);
#2739=EDGE_CURVE('',#2208,#2211,#1501,.T.);
#2740=EDGE_CURVE('',#2209,#2212,#1502,.T.);
#2741=EDGE_CURVE('',#2212,#2213,#1503,.T.);
#2742=EDGE_CURVE('',#2213,#2210,#1504,.T.);
#2743=EDGE_CURVE('',#2212,#2214,#1505,.T.);
#2744=EDGE_CURVE('',#2214,#2215,#1506,.T.);
#2745=EDGE_CURVE('',#2215,#2213,#1507,.T.);
#2746=EDGE_CURVE('',#2214,#2216,#1508,.T.);
#2747=EDGE_CURVE('',#2216,#2217,#1509,.T.);
#2748=EDGE_CURVE('',#2217,#2215,#1510,.T.);
#2749=EDGE_CURVE('',#2216,#2218,#1511,.T.);
#2750=EDGE_CURVE('',#2218,#2219,#1512,.T.);
#2751=EDGE_CURVE('',#2219,#2217,#1513,.T.);
#2752=EDGE_CURVE('',#2218,#2208,#1514,.T.);
#2753=EDGE_CURVE('',#2211,#2219,#1515,.T.);
#2754=ORIENTED_EDGE('',*,*,#2220,.F.);
#2755=ORIENTED_EDGE('',*,*,#2221,.T.);
#2756=ORIENTED_EDGE('',*,*,#2222,.F.);
#2757=ORIENTED_EDGE('',*,*,#2223,.F.);
#2758=ORIENTED_EDGE('',*,*,#2224,.F.);
#2759=ORIENTED_EDGE('',*,*,#2225,.T.);
#2760=ORIENTED_EDGE('',*,*,#2226,.F.);
#2761=ORIENTED_EDGE('',*,*,#2221,.F.);
#2762=ORIENTED_EDGE('',*,*,#2227,.F.);
#2763=ORIENTED_EDGE('',*,*,#2228,.T.);
#2764=ORIENTED_EDGE('',*,*,#2229,.F.);
#2765=ORIENTED_EDGE('',*,*,#2225,.F.);
#2766=ORIENTED_EDGE('',*,*,#2230,.F.);
#2767=ORIENTED_EDGE('',*,*,#2231,.T.);
#2768=ORIENTED_EDGE('',*,*,#2232,.F.);
#2769=ORIENTED_EDGE('',*,*,#2228,.F.);
#2770=ORIENTED_EDGE('',*,*,#2233,.F.);
#2771=ORIENTED_EDGE('',*,*,#2234,.T.);
#2772=ORIENTED_EDGE('',*,*,#2235,.F.);
#2773=ORIENTED_EDGE('',*,*,#2231,.F.);
#2774=ORIENTED_EDGE('',*,*,#2236,.F.);
#2775=ORIENTED_EDGE('',*,*,#2237,.T.);
#2776=ORIENTED_EDGE('',*,*,#2238,.F.);
#2777=ORIENTED_EDGE('',*,*,#2234,.F.);
#2778=ORIENTED_EDGE('',*,*,#2239,.F.);
#2779=ORIENTED_EDGE('',*,*,#2240,.T.);
#2780=ORIENTED_EDGE('',*,*,#2241,.F.);
#2781=ORIENTED_EDGE('',*,*,#2237,.F.);
#2782=ORIENTED_EDGE('',*,*,#2242,.F.);
#2783=ORIENTED_EDGE('',*,*,#2243,.T.);
#2784=ORIENTED_EDGE('',*,*,#2244,.F.);
#2785=ORIENTED_EDGE('',*,*,#2240,.F.);
#2786=ORIENTED_EDGE('',*,*,#2245,.F.);
#2787=ORIENTED_EDGE('',*,*,#2246,.F.);
#2788=ORIENTED_EDGE('',*,*,#2247,.F.);
#2789=ORIENTED_EDGE('',*,*,#2243,.F.);
#2790=ORIENTED_EDGE('',*,*,#2248,.F.);
#2791=ORIENTED_EDGE('',*,*,#2249,.T.);
#2792=ORIENTED_EDGE('',*,*,#2250,.F.);
#2793=ORIENTED_EDGE('',*,*,#2251,.F.);
#2794=ORIENTED_EDGE('',*,*,#2252,.F.);
#2795=ORIENTED_EDGE('',*,*,#2253,.T.);
#2796=ORIENTED_EDGE('',*,*,#2254,.F.);
#2797=ORIENTED_EDGE('',*,*,#2249,.F.);
#2798=ORIENTED_EDGE('',*,*,#2255,.F.);
#2799=ORIENTED_EDGE('',*,*,#2256,.T.);
#2800=ORIENTED_EDGE('',*,*,#2257,.F.);
#2801=ORIENTED_EDGE('',*,*,#2253,.F.);
#2802=ORIENTED_EDGE('',*,*,#2258,.F.);
#2803=ORIENTED_EDGE('',*,*,#2259,.T.);
#2804=ORIENTED_EDGE('',*,*,#2260,.F.);
#2805=ORIENTED_EDGE('',*,*,#2256,.F.);
#2806=ORIENTED_EDGE('',*,*,#2261,.F.);
#2807=ORIENTED_EDGE('',*,*,#2262,.T.);
#2808=ORIENTED_EDGE('',*,*,#2263,.F.);
#2809=ORIENTED_EDGE('',*,*,#2259,.F.);
#2810=ORIENTED_EDGE('',*,*,#2264,.F.);
#2811=ORIENTED_EDGE('',*,*,#2265,.T.);
#2812=ORIENTED_EDGE('',*,*,#2266,.F.);
#2813=ORIENTED_EDGE('',*,*,#2262,.F.);
#2814=ORIENTED_EDGE('',*,*,#2267,.F.);
#2815=ORIENTED_EDGE('',*,*,#2268,.T.);
#2816=ORIENTED_EDGE('',*,*,#2269,.F.);
#2817=ORIENTED_EDGE('',*,*,#2265,.F.);
#2818=ORIENTED_EDGE('',*,*,#2270,.F.);
#2819=ORIENTED_EDGE('',*,*,#2271,.T.);
#2820=ORIENTED_EDGE('',*,*,#2272,.F.);
#2821=ORIENTED_EDGE('',*,*,#2268,.F.);
#2822=ORIENTED_EDGE('',*,*,#2273,.F.);
#2823=ORIENTED_EDGE('',*,*,#2274,.F.);
#2824=ORIENTED_EDGE('',*,*,#2275,.F.);
#2825=ORIENTED_EDGE('',*,*,#2271,.F.);
#2826=ORIENTED_EDGE('',*,*,#2276,.F.);
#2827=ORIENTED_EDGE('',*,*,#2277,.T.);
#2828=ORIENTED_EDGE('',*,*,#2278,.F.);
#2829=ORIENTED_EDGE('',*,*,#2279,.F.);
#2830=ORIENTED_EDGE('',*,*,#2280,.F.);
#2831=ORIENTED_EDGE('',*,*,#2281,.T.);
#2832=ORIENTED_EDGE('',*,*,#2282,.F.);
#2833=ORIENTED_EDGE('',*,*,#2277,.F.);
#2834=ORIENTED_EDGE('',*,*,#2283,.F.);
#2835=ORIENTED_EDGE('',*,*,#2284,.T.);
#2836=ORIENTED_EDGE('',*,*,#2285,.F.);
#2837=ORIENTED_EDGE('',*,*,#2281,.F.);
#2838=ORIENTED_EDGE('',*,*,#2286,.F.);
#2839=ORIENTED_EDGE('',*,*,#2287,.T.);
#2840=ORIENTED_EDGE('',*,*,#2288,.F.);
#2841=ORIENTED_EDGE('',*,*,#2284,.F.);
#2842=ORIENTED_EDGE('',*,*,#2289,.F.);
#2843=ORIENTED_EDGE('',*,*,#2290,.T.);
#2844=ORIENTED_EDGE('',*,*,#2291,.F.);
#2845=ORIENTED_EDGE('',*,*,#2287,.F.);
#2846=ORIENTED_EDGE('',*,*,#2292,.F.);
#2847=ORIENTED_EDGE('',*,*,#2293,.T.);
#2848=ORIENTED_EDGE('',*,*,#2294,.F.);
#2849=ORIENTED_EDGE('',*,*,#2290,.F.);
#2850=ORIENTED_EDGE('',*,*,#2295,.F.);
#2851=ORIENTED_EDGE('',*,*,#2296,.T.);
#2852=ORIENTED_EDGE('',*,*,#2297,.F.);
#2853=ORIENTED_EDGE('',*,*,#2293,.F.);
#2854=ORIENTED_EDGE('',*,*,#2298,.F.);
#2855=ORIENTED_EDGE('',*,*,#2299,.T.);
#2856=ORIENTED_EDGE('',*,*,#2300,.F.);
#2857=ORIENTED_EDGE('',*,*,#2296,.F.);
#2858=ORIENTED_EDGE('',*,*,#2301,.F.);
#2859=ORIENTED_EDGE('',*,*,#2302,.F.);
#2860=ORIENTED_EDGE('',*,*,#2303,.F.);
#2861=ORIENTED_EDGE('',*,*,#2299,.F.);
#2862=ORIENTED_EDGE('',*,*,#2304,.F.);
#2863=ORIENTED_EDGE('',*,*,#2305,.T.);
#2864=ORIENTED_EDGE('',*,*,#2306,.F.);
#2865=ORIENTED_EDGE('',*,*,#2307,.F.);
#2866=ORIENTED_EDGE('',*,*,#2308,.F.);
#2867=ORIENTED_EDGE('',*,*,#2309,.T.);
#2868=ORIENTED_EDGE('',*,*,#2310,.F.);
#2869=ORIENTED_EDGE('',*,*,#2305,.F.);
#2870=ORIENTED_EDGE('',*,*,#2311,.F.);
#2871=ORIENTED_EDGE('',*,*,#2312,.T.);
#2872=ORIENTED_EDGE('',*,*,#2313,.F.);
#2873=ORIENTED_EDGE('',*,*,#2309,.F.);
#2874=ORIENTED_EDGE('',*,*,#2314,.F.);
#2875=ORIENTED_EDGE('',*,*,#2315,.T.);
#2876=ORIENTED_EDGE('',*,*,#2316,.F.);
#2877=ORIENTED_EDGE('',*,*,#2312,.F.);
#2878=ORIENTED_EDGE('',*,*,#2317,.F.);
#2879=ORIENTED_EDGE('',*,*,#2318,.T.);
#2880=ORIENTED_EDGE('',*,*,#2319,.F.);
#2881=ORIENTED_EDGE('',*,*,#2315,.F.);
#2882=ORIENTED_EDGE('',*,*,#2320,.F.);
#2883=ORIENTED_EDGE('',*,*,#2321,.T.);
#2884=ORIENTED_EDGE('',*,*,#2322,.F.);
#2885=ORIENTED_EDGE('',*,*,#2318,.F.);
#2886=ORIENTED_EDGE('',*,*,#2323,.F.);
#2887=ORIENTED_EDGE('',*,*,#2324,.T.);
#2888=ORIENTED_EDGE('',*,*,#2325,.F.);
#2889=ORIENTED_EDGE('',*,*,#2321,.F.);
#2890=ORIENTED_EDGE('',*,*,#2326,.F.);
#2891=ORIENTED_EDGE('',*,*,#2327,.T.);
#2892=ORIENTED_EDGE('',*,*,#2328,.F.);
#2893=ORIENTED_EDGE('',*,*,#2324,.F.);
#2894=ORIENTED_EDGE('',*,*,#2329,.F.);
#2895=ORIENTED_EDGE('',*,*,#2330,.F.);
#2896=ORIENTED_EDGE('',*,*,#2331,.F.);
#2897=ORIENTED_EDGE('',*,*,#2327,.F.);
#2898=ORIENTED_EDGE('',*,*,#2332,.F.);
#2899=ORIENTED_EDGE('',*,*,#2333,.T.);
#2900=ORIENTED_EDGE('',*,*,#2334,.F.);
#2901=ORIENTED_EDGE('',*,*,#2333,.F.);
#2902=ORIENTED_EDGE('',*,*,#2246,.T.);
#2903=ORIENTED_EDGE('',*,*,#2335,.T.);
#2904=ORIENTED_EDGE('',*,*,#2336,.T.);
#2905=ORIENTED_EDGE('',*,*,#2337,.F.);
#2906=ORIENTED_EDGE('',*,*,#2223,.T.);
#2907=ORIENTED_EDGE('',*,*,#2338,.F.);
#2908=ORIENTED_EDGE('',*,*,#2339,.F.);
#2909=ORIENTED_EDGE('',*,*,#2340,.T.);
#2910=ORIENTED_EDGE('',*,*,#2274,.T.);
#2911=ORIENTED_EDGE('',*,*,#2341,.T.);
#2912=ORIENTED_EDGE('',*,*,#2339,.T.);
#2913=ORIENTED_EDGE('',*,*,#2342,.F.);
#2914=ORIENTED_EDGE('',*,*,#2251,.T.);
#2915=ORIENTED_EDGE('',*,*,#2343,.F.);
#2916=ORIENTED_EDGE('',*,*,#2344,.F.);
#2917=ORIENTED_EDGE('',*,*,#2345,.T.);
#2918=ORIENTED_EDGE('',*,*,#2302,.T.);
#2919=ORIENTED_EDGE('',*,*,#2346,.T.);
#2920=ORIENTED_EDGE('',*,*,#2344,.T.);
#2921=ORIENTED_EDGE('',*,*,#2347,.F.);
#2922=ORIENTED_EDGE('',*,*,#2279,.T.);
#2923=ORIENTED_EDGE('',*,*,#2348,.F.);
#2924=ORIENTED_EDGE('',*,*,#2349,.F.);
#2925=ORIENTED_EDGE('',*,*,#2350,.T.);
#2926=ORIENTED_EDGE('',*,*,#2330,.T.);
#2927=ORIENTED_EDGE('',*,*,#2351,.T.);
#2928=ORIENTED_EDGE('',*,*,#2349,.T.);
#2929=ORIENTED_EDGE('',*,*,#2352,.F.);
#2930=ORIENTED_EDGE('',*,*,#2307,.T.);
#2931=ORIENTED_EDGE('',*,*,#2353,.F.);
#2932=ORIENTED_EDGE('',*,*,#2336,.F.);
#2933=ORIENTED_EDGE('',*,*,#2354,.T.);
#2934=ORIENTED_EDGE('',*,*,#2222,.T.);
#2935=ORIENTED_EDGE('',*,*,#2226,.T.);
#2936=ORIENTED_EDGE('',*,*,#2229,.T.);
#2937=ORIENTED_EDGE('',*,*,#2232,.T.);
#2938=ORIENTED_EDGE('',*,*,#2235,.T.);
#2939=ORIENTED_EDGE('',*,*,#2238,.T.);
#2940=ORIENTED_EDGE('',*,*,#2241,.T.);
#2941=ORIENTED_EDGE('',*,*,#2244,.T.);
#2942=ORIENTED_EDGE('',*,*,#2247,.T.);
#2943=ORIENTED_EDGE('',*,*,#2337,.T.);
#2944=ORIENTED_EDGE('',*,*,#2353,.T.);
#2945=ORIENTED_EDGE('',*,*,#2306,.T.);
#2946=ORIENTED_EDGE('',*,*,#2310,.T.);
#2947=ORIENTED_EDGE('',*,*,#2313,.T.);
#2948=ORIENTED_EDGE('',*,*,#2316,.T.);
#2949=ORIENTED_EDGE('',*,*,#2319,.T.);
#2950=ORIENTED_EDGE('',*,*,#2322,.T.);
#2951=ORIENTED_EDGE('',*,*,#2325,.T.);
#2952=ORIENTED_EDGE('',*,*,#2328,.T.);
#2953=ORIENTED_EDGE('',*,*,#2331,.T.);
#2954=ORIENTED_EDGE('',*,*,#2352,.T.);
#2955=ORIENTED_EDGE('',*,*,#2348,.T.);
#2956=ORIENTED_EDGE('',*,*,#2278,.T.);
#2957=ORIENTED_EDGE('',*,*,#2282,.T.);
#2958=ORIENTED_EDGE('',*,*,#2285,.T.);
#2959=ORIENTED_EDGE('',*,*,#2288,.T.);
#2960=ORIENTED_EDGE('',*,*,#2291,.T.);
#2961=ORIENTED_EDGE('',*,*,#2294,.T.);
#2962=ORIENTED_EDGE('',*,*,#2297,.T.);
#2963=ORIENTED_EDGE('',*,*,#2300,.T.);
#2964=ORIENTED_EDGE('',*,*,#2303,.T.);
#2965=ORIENTED_EDGE('',*,*,#2347,.T.);
#2966=ORIENTED_EDGE('',*,*,#2343,.T.);
#2967=ORIENTED_EDGE('',*,*,#2250,.T.);
#2968=ORIENTED_EDGE('',*,*,#2254,.T.);
#2969=ORIENTED_EDGE('',*,*,#2257,.T.);
#2970=ORIENTED_EDGE('',*,*,#2260,.T.);
#2971=ORIENTED_EDGE('',*,*,#2263,.T.);
#2972=ORIENTED_EDGE('',*,*,#2266,.T.);
#2973=ORIENTED_EDGE('',*,*,#2269,.T.);
#2974=ORIENTED_EDGE('',*,*,#2272,.T.);
#2975=ORIENTED_EDGE('',*,*,#2275,.T.);
#2976=ORIENTED_EDGE('',*,*,#2342,.T.);
#2977=ORIENTED_EDGE('',*,*,#2338,.T.);
#2978=ORIENTED_EDGE('',*,*,#2334,.T.);
#2979=ORIENTED_EDGE('',*,*,#2220,.T.);
#2980=ORIENTED_EDGE('',*,*,#2340,.F.);
#2981=ORIENTED_EDGE('',*,*,#2341,.F.);
#2982=ORIENTED_EDGE('',*,*,#2273,.T.);
#2983=ORIENTED_EDGE('',*,*,#2270,.T.);
#2984=ORIENTED_EDGE('',*,*,#2267,.T.);
#2985=ORIENTED_EDGE('',*,*,#2264,.T.);
#2986=ORIENTED_EDGE('',*,*,#2261,.T.);
#2987=ORIENTED_EDGE('',*,*,#2258,.T.);
#2988=ORIENTED_EDGE('',*,*,#2255,.T.);
#2989=ORIENTED_EDGE('',*,*,#2252,.T.);
#2990=ORIENTED_EDGE('',*,*,#2248,.T.);
#2991=ORIENTED_EDGE('',*,*,#2345,.F.);
#2992=ORIENTED_EDGE('',*,*,#2346,.F.);
#2993=ORIENTED_EDGE('',*,*,#2301,.T.);
#2994=ORIENTED_EDGE('',*,*,#2298,.T.);
#2995=ORIENTED_EDGE('',*,*,#2295,.T.);
#2996=ORIENTED_EDGE('',*,*,#2292,.T.);
#2997=ORIENTED_EDGE('',*,*,#2289,.T.);
#2998=ORIENTED_EDGE('',*,*,#2286,.T.);
#2999=ORIENTED_EDGE('',*,*,#2283,.T.);
#3000=ORIENTED_EDGE('',*,*,#2280,.T.);
#3001=ORIENTED_EDGE('',*,*,#2276,.T.);
#3002=ORIENTED_EDGE('',*,*,#2350,.F.);
#3003=ORIENTED_EDGE('',*,*,#2351,.F.);
#3004=ORIENTED_EDGE('',*,*,#2329,.T.);
#3005=ORIENTED_EDGE('',*,*,#2326,.T.);
#3006=ORIENTED_EDGE('',*,*,#2323,.T.);
#3007=ORIENTED_EDGE('',*,*,#2320,.T.);
#3008=ORIENTED_EDGE('',*,*,#2317,.T.);
#3009=ORIENTED_EDGE('',*,*,#2314,.T.);
#3010=ORIENTED_EDGE('',*,*,#2311,.T.);
#3011=ORIENTED_EDGE('',*,*,#2308,.T.);
#3012=ORIENTED_EDGE('',*,*,#2304,.T.);
#3013=ORIENTED_EDGE('',*,*,#2354,.F.);
#3014=ORIENTED_EDGE('',*,*,#2335,.F.);
#3015=ORIENTED_EDGE('',*,*,#2245,.T.);
#3016=ORIENTED_EDGE('',*,*,#2242,.T.);
#3017=ORIENTED_EDGE('',*,*,#2239,.T.);
#3018=ORIENTED_EDGE('',*,*,#2236,.T.);
#3019=ORIENTED_EDGE('',*,*,#2233,.T.);
#3020=ORIENTED_EDGE('',*,*,#2230,.T.);
#3021=ORIENTED_EDGE('',*,*,#2227,.T.);
#3022=ORIENTED_EDGE('',*,*,#2224,.T.);
#3023=ORIENTED_EDGE('',*,*,#2332,.T.);
#3024=ORIENTED_EDGE('',*,*,#2355,.F.);
#3025=ORIENTED_EDGE('',*,*,#2356,.T.);
#3026=ORIENTED_EDGE('',*,*,#2357,.F.);
#3027=ORIENTED_EDGE('',*,*,#2356,.F.);
#3028=ORIENTED_EDGE('',*,*,#2355,.T.);
#3029=ORIENTED_EDGE('',*,*,#2358,.F.);
#3030=ORIENTED_EDGE('',*,*,#2359,.T.);
#3031=ORIENTED_EDGE('',*,*,#2360,.T.);
#3032=ORIENTED_EDGE('',*,*,#2359,.F.);
#3033=ORIENTED_EDGE('',*,*,#2360,.F.);
#3034=ORIENTED_EDGE('',*,*,#2361,.T.);
#3035=ORIENTED_EDGE('',*,*,#2362,.F.);
#3036=ORIENTED_EDGE('',*,*,#2363,.F.);
#3037=ORIENTED_EDGE('',*,*,#2364,.F.);
#3038=ORIENTED_EDGE('',*,*,#2361,.F.);
#3039=ORIENTED_EDGE('',*,*,#2365,.T.);
#3040=ORIENTED_EDGE('',*,*,#2363,.T.);
#3041=ORIENTED_EDGE('',*,*,#2365,.F.);
#3042=ORIENTED_EDGE('',*,*,#2364,.T.);
#3043=ORIENTED_EDGE('',*,*,#2366,.T.);
#3044=ORIENTED_EDGE('',*,*,#2367,.T.);
#3045=ORIENTED_EDGE('',*,*,#2366,.F.);
#3046=ORIENTED_EDGE('',*,*,#2368,.F.);
#3047=ORIENTED_EDGE('',*,*,#2369,.T.);
#3048=ORIENTED_EDGE('',*,*,#2362,.T.);
#3049=ORIENTED_EDGE('',*,*,#2369,.F.);
#3050=ORIENTED_EDGE('',*,*,#2368,.T.);
#3051=ORIENTED_EDGE('',*,*,#2357,.T.);
#3052=ORIENTED_EDGE('',*,*,#2367,.F.);
#3053=ORIENTED_EDGE('',*,*,#2358,.T.);
#3054=ORIENTED_EDGE('',*,*,#2370,.F.);
#3055=ORIENTED_EDGE('',*,*,#2371,.F.);
#3056=ORIENTED_EDGE('',*,*,#2372,.F.);
#3057=ORIENTED_EDGE('',*,*,#2373,.F.);
#3058=ORIENTED_EDGE('',*,*,#2374,.F.);
#3059=ORIENTED_EDGE('',*,*,#2375,.F.);
#3060=ORIENTED_EDGE('',*,*,#2376,.F.);
#3061=ORIENTED_EDGE('',*,*,#2377,.F.);
#3062=ORIENTED_EDGE('',*,*,#2378,.F.);
#3063=ORIENTED_EDGE('',*,*,#2373,.T.);
#3064=ORIENTED_EDGE('',*,*,#2379,.F.);
#3065=ORIENTED_EDGE('',*,*,#2375,.T.);
#3066=ORIENTED_EDGE('',*,*,#2380,.F.);
#3067=ORIENTED_EDGE('',*,*,#2381,.F.);
#3068=ORIENTED_EDGE('',*,*,#2382,.F.);
#3069=ORIENTED_EDGE('',*,*,#2383,.F.);
#3070=ORIENTED_EDGE('',*,*,#2384,.F.);
#3071=ORIENTED_EDGE('',*,*,#2385,.F.);
#3072=ORIENTED_EDGE('',*,*,#2386,.F.);
#3073=ORIENTED_EDGE('',*,*,#2387,.F.);
#3074=ORIENTED_EDGE('',*,*,#2388,.F.);
#3075=ORIENTED_EDGE('',*,*,#2389,.F.);
#3076=ORIENTED_EDGE('',*,*,#2384,.T.);
#3077=ORIENTED_EDGE('',*,*,#2390,.F.);
#3078=ORIENTED_EDGE('',*,*,#2386,.T.);
#3079=ORIENTED_EDGE('',*,*,#2391,.F.);
#3080=ORIENTED_EDGE('',*,*,#2376,.T.);
#3081=ORIENTED_EDGE('',*,*,#2379,.T.);
#3082=ORIENTED_EDGE('',*,*,#2372,.T.);
#3083=ORIENTED_EDGE('',*,*,#2392,.F.);
#3084=ORIENTED_EDGE('',*,*,#2393,.F.);
#3085=ORIENTED_EDGE('',*,*,#2394,.T.);
#3086=ORIENTED_EDGE('',*,*,#2395,.T.);
#3087=ORIENTED_EDGE('',*,*,#2396,.F.);
#3088=ORIENTED_EDGE('',*,*,#2387,.T.);
#3089=ORIENTED_EDGE('',*,*,#2390,.T.);
#3090=ORIENTED_EDGE('',*,*,#2383,.T.);
#3091=ORIENTED_EDGE('',*,*,#2397,.F.);
#3092=ORIENTED_EDGE('',*,*,#2398,.T.);
#3093=ORIENTED_EDGE('',*,*,#2388,.T.);
#3094=ORIENTED_EDGE('',*,*,#2396,.T.);
#3095=ORIENTED_EDGE('',*,*,#2399,.T.);
#3096=ORIENTED_EDGE('',*,*,#2400,.T.);
#3097=ORIENTED_EDGE('',*,*,#2371,.T.);
#3098=ORIENTED_EDGE('',*,*,#2401,.T.);
#3099=ORIENTED_EDGE('',*,*,#2402,.T.);
#3100=ORIENTED_EDGE('',*,*,#2392,.T.);
#3101=ORIENTED_EDGE('',*,*,#2377,.T.);
#3102=ORIENTED_EDGE('',*,*,#2397,.T.);
#3103=ORIENTED_EDGE('',*,*,#2382,.T.);
#3104=ORIENTED_EDGE('',*,*,#2403,.T.);
#3105=ORIENTED_EDGE('',*,*,#2404,.F.);
#3106=ORIENTED_EDGE('',*,*,#2405,.T.);
#3107=ORIENTED_EDGE('',*,*,#2380,.T.);
#3108=ORIENTED_EDGE('',*,*,#2405,.F.);
#3109=ORIENTED_EDGE('',*,*,#2406,.F.);
#3110=ORIENTED_EDGE('',*,*,#2407,.T.);
#3111=ORIENTED_EDGE('',*,*,#2391,.T.);
#3112=ORIENTED_EDGE('',*,*,#2407,.F.);
#3113=ORIENTED_EDGE('',*,*,#2398,.F.);
#3114=ORIENTED_EDGE('',*,*,#2408,.T.);
#3115=ORIENTED_EDGE('',*,*,#2409,.F.);
#3116=ORIENTED_EDGE('',*,*,#2408,.F.);
#3117=ORIENTED_EDGE('',*,*,#2394,.F.);
#3118=ORIENTED_EDGE('',*,*,#2410,.F.);
#3119=ORIENTED_EDGE('',*,*,#2411,.F.);
#3120=ORIENTED_EDGE('',*,*,#2412,.T.);
#3121=ORIENTED_EDGE('',*,*,#2413,.F.);
#3122=ORIENTED_EDGE('',*,*,#2414,.T.);
#3123=ORIENTED_EDGE('',*,*,#2415,.F.);
#3124=ORIENTED_EDGE('',*,*,#2416,.F.);
#3125=ORIENTED_EDGE('',*,*,#2415,.T.);
#3126=ORIENTED_EDGE('',*,*,#2417,.T.);
#3127=ORIENTED_EDGE('',*,*,#2418,.T.);
#3128=ORIENTED_EDGE('',*,*,#2419,.T.);
#3129=ORIENTED_EDGE('',*,*,#2411,.T.);
#3130=ORIENTED_EDGE('',*,*,#2420,.T.);
#3131=ORIENTED_EDGE('',*,*,#2421,.T.);
#3132=ORIENTED_EDGE('',*,*,#2422,.T.);
#3133=ORIENTED_EDGE('',*,*,#2374,.T.);
#3134=ORIENTED_EDGE('',*,*,#2403,.F.);
#3135=ORIENTED_EDGE('',*,*,#2381,.T.);
#3136=ORIENTED_EDGE('',*,*,#2389,.T.);
#3137=ORIENTED_EDGE('',*,*,#2385,.T.);
#3138=ORIENTED_EDGE('',*,*,#2400,.F.);
#3139=ORIENTED_EDGE('',*,*,#2423,.F.);
#3140=ORIENTED_EDGE('',*,*,#2413,.T.);
#3141=ORIENTED_EDGE('',*,*,#2424,.T.);
#3142=ORIENTED_EDGE('',*,*,#2401,.F.);
#3143=ORIENTED_EDGE('',*,*,#2370,.T.);
#3144=ORIENTED_EDGE('',*,*,#2378,.T.);
#3145=ORIENTED_EDGE('',*,*,#2409,.T.);
#3146=ORIENTED_EDGE('',*,*,#2393,.T.);
#3147=ORIENTED_EDGE('',*,*,#2402,.F.);
#3148=ORIENTED_EDGE('',*,*,#2424,.F.);
#3149=ORIENTED_EDGE('',*,*,#2416,.T.);
#3150=ORIENTED_EDGE('',*,*,#2419,.F.);
#3151=ORIENTED_EDGE('',*,*,#2425,.T.);
#3152=ORIENTED_EDGE('',*,*,#2420,.F.);
#3153=ORIENTED_EDGE('',*,*,#2410,.T.);
#3154=ORIENTED_EDGE('',*,*,#2423,.T.);
#3155=ORIENTED_EDGE('',*,*,#2399,.F.);
#3156=ORIENTED_EDGE('',*,*,#2395,.F.);
#3157=ORIENTED_EDGE('',*,*,#2412,.F.);
#3158=ORIENTED_EDGE('',*,*,#2422,.F.);
#3159=ORIENTED_EDGE('',*,*,#2426,.T.);
#3160=ORIENTED_EDGE('',*,*,#2417,.F.);
#3161=ORIENTED_EDGE('',*,*,#2414,.F.);
#3162=ORIENTED_EDGE('',*,*,#2425,.F.);
#3163=ORIENTED_EDGE('',*,*,#2418,.F.);
#3164=ORIENTED_EDGE('',*,*,#2426,.F.);
#3165=ORIENTED_EDGE('',*,*,#2421,.F.);
#3166=ORIENTED_EDGE('',*,*,#2404,.T.);
#3167=ORIENTED_EDGE('',*,*,#2406,.T.);
#3168=ORIENTED_EDGE('',*,*,#2427,.F.);
#3169=ORIENTED_EDGE('',*,*,#2428,.F.);
#3170=ORIENTED_EDGE('',*,*,#2429,.F.);
#3171=ORIENTED_EDGE('',*,*,#2430,.F.);
#3172=ORIENTED_EDGE('',*,*,#2431,.F.);
#3173=ORIENTED_EDGE('',*,*,#2432,.F.);
#3174=ORIENTED_EDGE('',*,*,#2433,.F.);
#3175=ORIENTED_EDGE('',*,*,#2434,.F.);
#3176=ORIENTED_EDGE('',*,*,#2435,.F.);
#3177=ORIENTED_EDGE('',*,*,#2430,.T.);
#3178=ORIENTED_EDGE('',*,*,#2436,.F.);
#3179=ORIENTED_EDGE('',*,*,#2432,.T.);
#3180=ORIENTED_EDGE('',*,*,#2437,.F.);
#3181=ORIENTED_EDGE('',*,*,#2438,.F.);
#3182=ORIENTED_EDGE('',*,*,#2439,.F.);
#3183=ORIENTED_EDGE('',*,*,#2440,.F.);
#3184=ORIENTED_EDGE('',*,*,#2441,.F.);
#3185=ORIENTED_EDGE('',*,*,#2442,.F.);
#3186=ORIENTED_EDGE('',*,*,#2443,.F.);
#3187=ORIENTED_EDGE('',*,*,#2444,.F.);
#3188=ORIENTED_EDGE('',*,*,#2445,.F.);
#3189=ORIENTED_EDGE('',*,*,#2446,.F.);
#3190=ORIENTED_EDGE('',*,*,#2441,.T.);
#3191=ORIENTED_EDGE('',*,*,#2447,.F.);
#3192=ORIENTED_EDGE('',*,*,#2443,.T.);
#3193=ORIENTED_EDGE('',*,*,#2448,.F.);
#3194=ORIENTED_EDGE('',*,*,#2433,.T.);
#3195=ORIENTED_EDGE('',*,*,#2436,.T.);
#3196=ORIENTED_EDGE('',*,*,#2429,.T.);
#3197=ORIENTED_EDGE('',*,*,#2449,.F.);
#3198=ORIENTED_EDGE('',*,*,#2450,.F.);
#3199=ORIENTED_EDGE('',*,*,#2451,.T.);
#3200=ORIENTED_EDGE('',*,*,#2452,.T.);
#3201=ORIENTED_EDGE('',*,*,#2453,.F.);
#3202=ORIENTED_EDGE('',*,*,#2444,.T.);
#3203=ORIENTED_EDGE('',*,*,#2447,.T.);
#3204=ORIENTED_EDGE('',*,*,#2440,.T.);
#3205=ORIENTED_EDGE('',*,*,#2454,.F.);
#3206=ORIENTED_EDGE('',*,*,#2455,.T.);
#3207=ORIENTED_EDGE('',*,*,#2445,.T.);
#3208=ORIENTED_EDGE('',*,*,#2453,.T.);
#3209=ORIENTED_EDGE('',*,*,#2456,.T.);
#3210=ORIENTED_EDGE('',*,*,#2457,.T.);
#3211=ORIENTED_EDGE('',*,*,#2428,.T.);
#3212=ORIENTED_EDGE('',*,*,#2458,.T.);
#3213=ORIENTED_EDGE('',*,*,#2459,.T.);
#3214=ORIENTED_EDGE('',*,*,#2449,.T.);
#3215=ORIENTED_EDGE('',*,*,#2434,.T.);
#3216=ORIENTED_EDGE('',*,*,#2454,.T.);
#3217=ORIENTED_EDGE('',*,*,#2439,.T.);
#3218=ORIENTED_EDGE('',*,*,#2460,.T.);
#3219=ORIENTED_EDGE('',*,*,#2461,.F.);
#3220=ORIENTED_EDGE('',*,*,#2462,.T.);
#3221=ORIENTED_EDGE('',*,*,#2437,.T.);
#3222=ORIENTED_EDGE('',*,*,#2462,.F.);
#3223=ORIENTED_EDGE('',*,*,#2463,.F.);
#3224=ORIENTED_EDGE('',*,*,#2464,.T.);
#3225=ORIENTED_EDGE('',*,*,#2448,.T.);
#3226=ORIENTED_EDGE('',*,*,#2464,.F.);
#3227=ORIENTED_EDGE('',*,*,#2455,.F.);
#3228=ORIENTED_EDGE('',*,*,#2465,.T.);
#3229=ORIENTED_EDGE('',*,*,#2466,.F.);
#3230=ORIENTED_EDGE('',*,*,#2465,.F.);
#3231=ORIENTED_EDGE('',*,*,#2451,.F.);
#3232=ORIENTED_EDGE('',*,*,#2467,.F.);
#3233=ORIENTED_EDGE('',*,*,#2468,.F.);
#3234=ORIENTED_EDGE('',*,*,#2469,.T.);
#3235=ORIENTED_EDGE('',*,*,#2470,.F.);
#3236=ORIENTED_EDGE('',*,*,#2471,.T.);
#3237=ORIENTED_EDGE('',*,*,#2472,.F.);
#3238=ORIENTED_EDGE('',*,*,#2473,.F.);
#3239=ORIENTED_EDGE('',*,*,#2472,.T.);
#3240=ORIENTED_EDGE('',*,*,#2474,.T.);
#3241=ORIENTED_EDGE('',*,*,#2475,.T.);
#3242=ORIENTED_EDGE('',*,*,#2476,.T.);
#3243=ORIENTED_EDGE('',*,*,#2468,.T.);
#3244=ORIENTED_EDGE('',*,*,#2477,.T.);
#3245=ORIENTED_EDGE('',*,*,#2478,.T.);
#3246=ORIENTED_EDGE('',*,*,#2479,.T.);
#3247=ORIENTED_EDGE('',*,*,#2431,.T.);
#3248=ORIENTED_EDGE('',*,*,#2460,.F.);
#3249=ORIENTED_EDGE('',*,*,#2438,.T.);
#3250=ORIENTED_EDGE('',*,*,#2446,.T.);
#3251=ORIENTED_EDGE('',*,*,#2442,.T.);
#3252=ORIENTED_EDGE('',*,*,#2457,.F.);
#3253=ORIENTED_EDGE('',*,*,#2480,.F.);
#3254=ORIENTED_EDGE('',*,*,#2470,.T.);
#3255=ORIENTED_EDGE('',*,*,#2481,.T.);
#3256=ORIENTED_EDGE('',*,*,#2458,.F.);
#3257=ORIENTED_EDGE('',*,*,#2427,.T.);
#3258=ORIENTED_EDGE('',*,*,#2435,.T.);
#3259=ORIENTED_EDGE('',*,*,#2466,.T.);
#3260=ORIENTED_EDGE('',*,*,#2450,.T.);
#3261=ORIENTED_EDGE('',*,*,#2459,.F.);
#3262=ORIENTED_EDGE('',*,*,#2481,.F.);
#3263=ORIENTED_EDGE('',*,*,#2473,.T.);
#3264=ORIENTED_EDGE('',*,*,#2476,.F.);
#3265=ORIENTED_EDGE('',*,*,#2482,.T.);
#3266=ORIENTED_EDGE('',*,*,#2477,.F.);
#3267=ORIENTED_EDGE('',*,*,#2467,.T.);
#3268=ORIENTED_EDGE('',*,*,#2480,.T.);
#3269=ORIENTED_EDGE('',*,*,#2456,.F.);
#3270=ORIENTED_EDGE('',*,*,#2452,.F.);
#3271=ORIENTED_EDGE('',*,*,#2469,.F.);
#3272=ORIENTED_EDGE('',*,*,#2479,.F.);
#3273=ORIENTED_EDGE('',*,*,#2483,.T.);
#3274=ORIENTED_EDGE('',*,*,#2474,.F.);
#3275=ORIENTED_EDGE('',*,*,#2471,.F.);
#3276=ORIENTED_EDGE('',*,*,#2482,.F.);
#3277=ORIENTED_EDGE('',*,*,#2475,.F.);
#3278=ORIENTED_EDGE('',*,*,#2483,.F.);
#3279=ORIENTED_EDGE('',*,*,#2478,.F.);
#3280=ORIENTED_EDGE('',*,*,#2461,.T.);
#3281=ORIENTED_EDGE('',*,*,#2463,.T.);
#3282=ORIENTED_EDGE('',*,*,#2484,.T.);
#3283=ORIENTED_EDGE('',*,*,#2485,.T.);
#3284=ORIENTED_EDGE('',*,*,#2486,.T.);
#3285=ORIENTED_EDGE('',*,*,#2487,.F.);
#3286=ORIENTED_EDGE('',*,*,#2488,.T.);
#3287=ORIENTED_EDGE('',*,*,#2489,.T.);
#3288=ORIENTED_EDGE('',*,*,#2490,.T.);
#3289=ORIENTED_EDGE('',*,*,#2485,.F.);
#3290=ORIENTED_EDGE('',*,*,#2491,.T.);
#3291=ORIENTED_EDGE('',*,*,#2492,.T.);
#3292=ORIENTED_EDGE('',*,*,#2493,.T.);
#3293=ORIENTED_EDGE('',*,*,#2489,.F.);
#3294=ORIENTED_EDGE('',*,*,#2494,.T.);
#3295=ORIENTED_EDGE('',*,*,#2495,.T.);
#3296=ORIENTED_EDGE('',*,*,#2496,.T.);
#3297=ORIENTED_EDGE('',*,*,#2492,.F.);
#3298=ORIENTED_EDGE('',*,*,#2497,.T.);
#3299=ORIENTED_EDGE('',*,*,#2498,.T.);
#3300=ORIENTED_EDGE('',*,*,#2499,.T.);
#3301=ORIENTED_EDGE('',*,*,#2495,.F.);
#3302=ORIENTED_EDGE('',*,*,#2500,.T.);
#3303=ORIENTED_EDGE('',*,*,#2487,.T.);
#3304=ORIENTED_EDGE('',*,*,#2501,.T.);
#3305=ORIENTED_EDGE('',*,*,#2498,.F.);
#3306=ORIENTED_EDGE('',*,*,#2500,.F.);
#3307=ORIENTED_EDGE('',*,*,#2497,.F.);
#3308=ORIENTED_EDGE('',*,*,#2494,.F.);
#3309=ORIENTED_EDGE('',*,*,#2491,.F.);
#3310=ORIENTED_EDGE('',*,*,#2488,.F.);
#3311=ORIENTED_EDGE('',*,*,#2484,.F.);
#3312=ORIENTED_EDGE('',*,*,#2501,.F.);
#3313=ORIENTED_EDGE('',*,*,#2486,.F.);
#3314=ORIENTED_EDGE('',*,*,#2490,.F.);
#3315=ORIENTED_EDGE('',*,*,#2493,.F.);
#3316=ORIENTED_EDGE('',*,*,#2496,.F.);
#3317=ORIENTED_EDGE('',*,*,#2499,.F.);
#3318=ORIENTED_EDGE('',*,*,#2502,.F.);
#3319=ORIENTED_EDGE('',*,*,#2503,.F.);
#3320=ORIENTED_EDGE('',*,*,#2504,.F.);
#3321=ORIENTED_EDGE('',*,*,#2505,.T.);
#3322=ORIENTED_EDGE('',*,*,#2503,.T.);
#3323=ORIENTED_EDGE('',*,*,#2505,.F.);
#3324=ORIENTED_EDGE('',*,*,#2506,.F.);
#3325=ORIENTED_EDGE('',*,*,#2507,.T.);
#3326=ORIENTED_EDGE('',*,*,#2504,.T.);
#3327=ORIENTED_EDGE('',*,*,#2507,.F.);
#3328=ORIENTED_EDGE('',*,*,#2508,.F.);
#3329=ORIENTED_EDGE('',*,*,#2509,.T.);
#3330=ORIENTED_EDGE('',*,*,#2506,.T.);
#3331=ORIENTED_EDGE('',*,*,#2509,.F.);
#3332=ORIENTED_EDGE('',*,*,#2508,.T.);
#3333=ORIENTED_EDGE('',*,*,#2510,.F.);
#3334=ORIENTED_EDGE('',*,*,#2511,.F.);
#3335=ORIENTED_EDGE('',*,*,#2512,.T.);
#3336=ORIENTED_EDGE('',*,*,#2510,.T.);
#3337=ORIENTED_EDGE('',*,*,#2512,.F.);
#3338=ORIENTED_EDGE('',*,*,#2502,.T.);
#3339=ORIENTED_EDGE('',*,*,#2513,.T.);
#3340=ORIENTED_EDGE('',*,*,#2511,.T.);
#3341=ORIENTED_EDGE('',*,*,#2513,.F.);
#3342=ORIENTED_EDGE('',*,*,#2514,.F.);
#3343=ORIENTED_EDGE('',*,*,#2515,.F.);
#3344=ORIENTED_EDGE('',*,*,#2516,.F.);
#3345=ORIENTED_EDGE('',*,*,#2517,.F.);
#3346=ORIENTED_EDGE('',*,*,#2516,.T.);
#3347=ORIENTED_EDGE('',*,*,#2518,.T.);
#3348=ORIENTED_EDGE('',*,*,#2519,.F.);
#3349=ORIENTED_EDGE('',*,*,#2520,.F.);
#3350=ORIENTED_EDGE('',*,*,#2521,.T.);
#3351=ORIENTED_EDGE('',*,*,#2522,.T.);
#3352=ORIENTED_EDGE('',*,*,#2523,.T.);
#3353=ORIENTED_EDGE('',*,*,#2519,.T.);
#3354=ORIENTED_EDGE('',*,*,#2524,.T.);
#3355=ORIENTED_EDGE('',*,*,#2521,.F.);
#3356=ORIENTED_EDGE('',*,*,#2518,.F.);
#3357=ORIENTED_EDGE('',*,*,#2515,.T.);
#3358=ORIENTED_EDGE('',*,*,#2525,.F.);
#3359=ORIENTED_EDGE('',*,*,#2526,.F.);
#3360=ORIENTED_EDGE('',*,*,#2527,.T.);
#3361=ORIENTED_EDGE('',*,*,#2528,.F.);
#3362=ORIENTED_EDGE('',*,*,#2529,.T.);
#3363=ORIENTED_EDGE('',*,*,#2530,.T.);
#3364=ORIENTED_EDGE('',*,*,#2531,.T.);
#3365=ORIENTED_EDGE('',*,*,#2532,.T.);
#3366=ORIENTED_EDGE('',*,*,#2533,.T.);
#3367=ORIENTED_EDGE('',*,*,#2522,.F.);
#3368=ORIENTED_EDGE('',*,*,#2531,.F.);
#3369=ORIENTED_EDGE('',*,*,#2534,.F.);
#3370=ORIENTED_EDGE('',*,*,#2535,.F.);
#3371=ORIENTED_EDGE('',*,*,#2532,.F.);
#3372=ORIENTED_EDGE('',*,*,#2530,.F.);
#3373=ORIENTED_EDGE('',*,*,#2523,.F.);
#3374=ORIENTED_EDGE('',*,*,#2533,.F.);
#3375=ORIENTED_EDGE('',*,*,#2535,.T.);
#3376=ORIENTED_EDGE('',*,*,#2536,.F.);
#3377=ORIENTED_EDGE('',*,*,#2537,.F.);
#3378=ORIENTED_EDGE('',*,*,#2538,.T.);
#3379=ORIENTED_EDGE('',*,*,#2539,.F.);
#3380=ORIENTED_EDGE('',*,*,#2540,.T.);
#3381=ORIENTED_EDGE('',*,*,#2517,.T.);
#3382=ORIENTED_EDGE('',*,*,#2520,.T.);
#3383=ORIENTED_EDGE('',*,*,#2534,.T.);
#3384=ORIENTED_EDGE('',*,*,#2529,.F.);
#3385=ORIENTED_EDGE('',*,*,#2541,.F.);
#3386=ORIENTED_EDGE('',*,*,#2536,.T.);
#3387=ORIENTED_EDGE('',*,*,#2537,.T.);
#3388=ORIENTED_EDGE('',*,*,#2541,.T.);
#3389=ORIENTED_EDGE('',*,*,#2528,.T.);
#3390=ORIENTED_EDGE('',*,*,#2542,.T.);
#3391=ORIENTED_EDGE('',*,*,#2543,.T.);
#3392=ORIENTED_EDGE('',*,*,#2544,.T.);
#3393=ORIENTED_EDGE('',*,*,#2543,.F.);
#3394=ORIENTED_EDGE('',*,*,#2545,.F.);
#3395=ORIENTED_EDGE('',*,*,#2546,.T.);
#3396=ORIENTED_EDGE('',*,*,#2524,.F.);
#3397=ORIENTED_EDGE('',*,*,#2546,.F.);
#3398=ORIENTED_EDGE('',*,*,#2547,.F.);
#3399=ORIENTED_EDGE('',*,*,#2548,.F.);
#3400=ORIENTED_EDGE('',*,*,#2549,.F.);
#3401=ORIENTED_EDGE('',*,*,#2542,.F.);
#3402=ORIENTED_EDGE('',*,*,#2527,.F.);
#3403=ORIENTED_EDGE('',*,*,#2550,.F.);
#3404=ORIENTED_EDGE('',*,*,#2547,.T.);
#3405=ORIENTED_EDGE('',*,*,#2545,.T.);
#3406=ORIENTED_EDGE('',*,*,#2544,.F.);
#3407=ORIENTED_EDGE('',*,*,#2549,.T.);
#3408=ORIENTED_EDGE('',*,*,#2551,.F.);
#3409=ORIENTED_EDGE('',*,*,#2538,.F.);
#3410=ORIENTED_EDGE('',*,*,#2526,.T.);
#3411=ORIENTED_EDGE('',*,*,#2552,.T.);
#3412=ORIENTED_EDGE('',*,*,#2539,.T.);
#3413=ORIENTED_EDGE('',*,*,#2551,.T.);
#3414=ORIENTED_EDGE('',*,*,#2548,.T.);
#3415=ORIENTED_EDGE('',*,*,#2550,.T.);
#3416=ORIENTED_EDGE('',*,*,#2514,.T.);
#3417=ORIENTED_EDGE('',*,*,#2540,.F.);
#3418=ORIENTED_EDGE('',*,*,#2552,.F.);
#3419=ORIENTED_EDGE('',*,*,#2525,.T.);
#3420=ORIENTED_EDGE('',*,*,#2553,.F.);
#3421=ORIENTED_EDGE('',*,*,#2554,.F.);
#3422=ORIENTED_EDGE('',*,*,#2555,.T.);
#3423=ORIENTED_EDGE('',*,*,#2556,.F.);
#3424=ORIENTED_EDGE('',*,*,#2557,.F.);
#3425=ORIENTED_EDGE('',*,*,#2555,.F.);
#3426=ORIENTED_EDGE('',*,*,#2556,.T.);
#3427=ORIENTED_EDGE('',*,*,#2557,.T.);
#3428=ORIENTED_EDGE('',*,*,#2558,.T.);
#3429=ORIENTED_EDGE('',*,*,#2559,.T.);
#3430=ORIENTED_EDGE('',*,*,#2558,.F.);
#3431=ORIENTED_EDGE('',*,*,#2560,.T.);
#3432=ORIENTED_EDGE('',*,*,#2561,.T.);
#3433=ORIENTED_EDGE('',*,*,#2562,.F.);
#3434=ORIENTED_EDGE('',*,*,#2561,.F.);
#3435=ORIENTED_EDGE('',*,*,#2562,.T.);
#3436=ORIENTED_EDGE('',*,*,#2563,.T.);
#3437=ORIENTED_EDGE('',*,*,#2564,.F.);
#3438=ORIENTED_EDGE('',*,*,#2563,.F.);
#3439=ORIENTED_EDGE('',*,*,#2559,.F.);
#3440=ORIENTED_EDGE('',*,*,#2564,.T.);
#3441=ORIENTED_EDGE('',*,*,#2565,.F.);
#3442=ORIENTED_EDGE('',*,*,#2566,.T.);
#3443=ORIENTED_EDGE('',*,*,#2553,.T.);
#3444=ORIENTED_EDGE('',*,*,#2554,.T.);
#3445=ORIENTED_EDGE('',*,*,#2566,.F.);
#3446=ORIENTED_EDGE('',*,*,#2565,.T.);
#3447=ORIENTED_EDGE('',*,*,#2567,.F.);
#3448=ORIENTED_EDGE('',*,*,#2567,.T.);
#3449=ORIENTED_EDGE('',*,*,#2568,.T.);
#3450=ORIENTED_EDGE('',*,*,#2560,.F.);
#3451=ORIENTED_EDGE('',*,*,#2568,.F.);
#3452=ORIENTED_EDGE('',*,*,#2569,.F.);
#3453=ORIENTED_EDGE('',*,*,#2570,.F.);
#3454=ORIENTED_EDGE('',*,*,#2571,.T.);
#3455=ORIENTED_EDGE('',*,*,#2572,.F.);
#3456=ORIENTED_EDGE('',*,*,#2573,.F.);
#3457=ORIENTED_EDGE('',*,*,#2571,.F.);
#3458=ORIENTED_EDGE('',*,*,#2574,.T.);
#3459=ORIENTED_EDGE('',*,*,#2575,.T.);
#3460=ORIENTED_EDGE('',*,*,#2572,.T.);
#3461=ORIENTED_EDGE('',*,*,#2573,.T.);
#3462=ORIENTED_EDGE('',*,*,#2575,.F.);
#3463=ORIENTED_EDGE('',*,*,#2576,.F.);
#3464=ORIENTED_EDGE('',*,*,#2577,.T.);
#3465=ORIENTED_EDGE('',*,*,#2578,.F.);
#3466=ORIENTED_EDGE('',*,*,#2579,.T.);
#3467=ORIENTED_EDGE('',*,*,#2576,.T.);
#3468=ORIENTED_EDGE('',*,*,#2579,.F.);
#3469=ORIENTED_EDGE('',*,*,#2580,.F.);
#3470=ORIENTED_EDGE('',*,*,#2581,.T.);
#3471=ORIENTED_EDGE('',*,*,#2578,.T.);
#3472=ORIENTED_EDGE('',*,*,#2581,.F.);
#3473=ORIENTED_EDGE('',*,*,#2582,.F.);
#3474=ORIENTED_EDGE('',*,*,#2583,.T.);
#3475=ORIENTED_EDGE('',*,*,#2580,.T.);
#3476=ORIENTED_EDGE('',*,*,#2583,.F.);
#3477=ORIENTED_EDGE('',*,*,#2582,.T.);
#3478=ORIENTED_EDGE('',*,*,#2574,.F.);
#3479=ORIENTED_EDGE('',*,*,#2569,.T.);
#3480=ORIENTED_EDGE('',*,*,#2570,.T.);
#3481=ORIENTED_EDGE('',*,*,#2584,.T.);
#3482=ORIENTED_EDGE('',*,*,#2577,.F.);
#3483=ORIENTED_EDGE('',*,*,#2584,.F.);
#3484=ORIENTED_EDGE('',*,*,#2585,.T.);
#3485=ORIENTED_EDGE('',*,*,#2585,.F.);
#3486=ORIENTED_EDGE('',*,*,#2586,.T.);
#3487=ORIENTED_EDGE('',*,*,#2586,.F.);
#3488=ORIENTED_EDGE('',*,*,#2587,.T.);
#3489=ORIENTED_EDGE('',*,*,#2587,.F.);
#3490=ORIENTED_EDGE('',*,*,#2588,.T.);
#3491=ORIENTED_EDGE('',*,*,#2588,.F.);
#3492=ORIENTED_EDGE('',*,*,#2589,.T.);
#3493=ORIENTED_EDGE('',*,*,#2589,.F.);
#3494=ORIENTED_EDGE('',*,*,#2590,.T.);
#3495=ORIENTED_EDGE('',*,*,#2590,.F.);
#3496=ORIENTED_EDGE('',*,*,#2591,.T.);
#3497=ORIENTED_EDGE('',*,*,#2591,.F.);
#3498=ORIENTED_EDGE('',*,*,#2592,.T.);
#3499=ORIENTED_EDGE('',*,*,#2592,.F.);
#3500=ORIENTED_EDGE('',*,*,#2593,.F.);
#3501=ORIENTED_EDGE('',*,*,#2594,.F.);
#3502=ORIENTED_EDGE('',*,*,#2595,.F.);
#3503=ORIENTED_EDGE('',*,*,#2596,.F.);
#3504=ORIENTED_EDGE('',*,*,#2595,.T.);
#3505=ORIENTED_EDGE('',*,*,#2597,.F.);
#3506=ORIENTED_EDGE('',*,*,#2598,.T.);
#3507=ORIENTED_EDGE('',*,*,#2599,.F.);
#3508=ORIENTED_EDGE('',*,*,#2600,.T.);
#3509=ORIENTED_EDGE('',*,*,#2601,.F.);
#3510=ORIENTED_EDGE('',*,*,#2602,.T.);
#3511=ORIENTED_EDGE('',*,*,#2603,.T.);
#3512=ORIENTED_EDGE('',*,*,#2604,.F.);
#3513=ORIENTED_EDGE('',*,*,#2603,.F.);
#3514=ORIENTED_EDGE('',*,*,#2605,.T.);
#3515=ORIENTED_EDGE('',*,*,#2606,.F.);
#3516=ORIENTED_EDGE('',*,*,#2607,.T.);
#3517=ORIENTED_EDGE('',*,*,#2608,.F.);
#3518=ORIENTED_EDGE('',*,*,#2609,.T.);
#3519=ORIENTED_EDGE('',*,*,#2610,.F.);
#3520=ORIENTED_EDGE('',*,*,#2611,.T.);
#3521=ORIENTED_EDGE('',*,*,#2612,.F.);
#3522=ORIENTED_EDGE('',*,*,#2613,.T.);
#3523=ORIENTED_EDGE('',*,*,#2614,.F.);
#3524=ORIENTED_EDGE('',*,*,#2594,.T.);
#3525=ORIENTED_EDGE('',*,*,#2615,.T.);
#3526=ORIENTED_EDGE('',*,*,#2616,.T.);
#3527=ORIENTED_EDGE('',*,*,#2597,.T.);
#3528=ORIENTED_EDGE('',*,*,#2617,.F.);
#3529=ORIENTED_EDGE('',*,*,#2618,.F.);
#3530=ORIENTED_EDGE('',*,*,#2598,.F.);
#3531=ORIENTED_EDGE('',*,*,#2616,.F.);
#3532=ORIENTED_EDGE('',*,*,#2618,.T.);
#3533=ORIENTED_EDGE('',*,*,#2619,.T.);
#3534=ORIENTED_EDGE('',*,*,#2620,.T.);
#3535=ORIENTED_EDGE('',*,*,#2599,.T.);
#3536=ORIENTED_EDGE('',*,*,#2621,.F.);
#3537=ORIENTED_EDGE('',*,*,#2622,.F.);
#3538=ORIENTED_EDGE('',*,*,#2600,.F.);
#3539=ORIENTED_EDGE('',*,*,#2620,.F.);
#3540=ORIENTED_EDGE('',*,*,#2622,.T.);
#3541=ORIENTED_EDGE('',*,*,#2623,.T.);
#3542=ORIENTED_EDGE('',*,*,#2624,.T.);
#3543=ORIENTED_EDGE('',*,*,#2601,.T.);
#3544=ORIENTED_EDGE('',*,*,#2625,.F.);
#3545=ORIENTED_EDGE('',*,*,#2626,.F.);
#3546=ORIENTED_EDGE('',*,*,#2605,.F.);
#3547=ORIENTED_EDGE('',*,*,#2602,.F.);
#3548=ORIENTED_EDGE('',*,*,#2624,.F.);
#3549=ORIENTED_EDGE('',*,*,#2627,.F.);
#3550=ORIENTED_EDGE('',*,*,#2626,.T.);
#3551=ORIENTED_EDGE('',*,*,#2628,.T.);
#3552=ORIENTED_EDGE('',*,*,#2629,.T.);
#3553=ORIENTED_EDGE('',*,*,#2606,.T.);
#3554=ORIENTED_EDGE('',*,*,#2630,.F.);
#3555=ORIENTED_EDGE('',*,*,#2631,.F.);
#3556=ORIENTED_EDGE('',*,*,#2607,.F.);
#3557=ORIENTED_EDGE('',*,*,#2629,.F.);
#3558=ORIENTED_EDGE('',*,*,#2631,.T.);
#3559=ORIENTED_EDGE('',*,*,#2632,.T.);
#3560=ORIENTED_EDGE('',*,*,#2633,.T.);
#3561=ORIENTED_EDGE('',*,*,#2608,.T.);
#3562=ORIENTED_EDGE('',*,*,#2634,.F.);
#3563=ORIENTED_EDGE('',*,*,#2635,.F.);
#3564=ORIENTED_EDGE('',*,*,#2609,.F.);
#3565=ORIENTED_EDGE('',*,*,#2633,.F.);
#3566=ORIENTED_EDGE('',*,*,#2635,.T.);
#3567=ORIENTED_EDGE('',*,*,#2636,.T.);
#3568=ORIENTED_EDGE('',*,*,#2637,.T.);
#3569=ORIENTED_EDGE('',*,*,#2610,.T.);
#3570=ORIENTED_EDGE('',*,*,#2611,.F.);
#3571=ORIENTED_EDGE('',*,*,#2637,.F.);
#3572=ORIENTED_EDGE('',*,*,#2638,.F.);
#3573=ORIENTED_EDGE('',*,*,#2639,.F.);
#3574=ORIENTED_EDGE('',*,*,#2640,.F.);
#3575=ORIENTED_EDGE('',*,*,#2641,.T.);
#3576=ORIENTED_EDGE('',*,*,#2627,.T.);
#3577=ORIENTED_EDGE('',*,*,#2623,.F.);
#3578=ORIENTED_EDGE('',*,*,#2621,.T.);
#3579=ORIENTED_EDGE('',*,*,#2619,.F.);
#3580=ORIENTED_EDGE('',*,*,#2617,.T.);
#3581=ORIENTED_EDGE('',*,*,#2615,.F.);
#3582=ORIENTED_EDGE('',*,*,#2593,.T.);
#3583=ORIENTED_EDGE('',*,*,#2642,.F.);
#3584=ORIENTED_EDGE('',*,*,#2643,.T.);
#3585=ORIENTED_EDGE('',*,*,#2644,.F.);
#3586=ORIENTED_EDGE('',*,*,#2638,.T.);
#3587=ORIENTED_EDGE('',*,*,#2636,.F.);
#3588=ORIENTED_EDGE('',*,*,#2634,.T.);
#3589=ORIENTED_EDGE('',*,*,#2632,.F.);
#3590=ORIENTED_EDGE('',*,*,#2630,.T.);
#3591=ORIENTED_EDGE('',*,*,#2628,.F.);
#3592=ORIENTED_EDGE('',*,*,#2625,.T.);
#3593=ORIENTED_EDGE('',*,*,#2641,.F.);
#3594=ORIENTED_EDGE('',*,*,#2596,.T.);
#3595=ORIENTED_EDGE('',*,*,#2614,.T.);
#3596=ORIENTED_EDGE('',*,*,#2645,.T.);
#3597=ORIENTED_EDGE('',*,*,#2642,.T.);
#3598=ORIENTED_EDGE('',*,*,#2613,.F.);
#3599=ORIENTED_EDGE('',*,*,#2646,.F.);
#3600=ORIENTED_EDGE('',*,*,#2643,.F.);
#3601=ORIENTED_EDGE('',*,*,#2645,.F.);
#3602=ORIENTED_EDGE('',*,*,#2604,.T.);
#3603=ORIENTED_EDGE('',*,*,#2640,.T.);
#3604=ORIENTED_EDGE('',*,*,#2639,.T.);
#3605=ORIENTED_EDGE('',*,*,#2644,.T.);
#3606=ORIENTED_EDGE('',*,*,#2646,.T.);
#3607=ORIENTED_EDGE('',*,*,#2612,.T.);
#3608=ORIENTED_EDGE('',*,*,#2647,.F.);
#3609=ORIENTED_EDGE('',*,*,#2648,.T.);
#3610=ORIENTED_EDGE('',*,*,#2649,.F.);
#3611=ORIENTED_EDGE('',*,*,#2650,.T.);
#3612=ORIENTED_EDGE('',*,*,#2647,.T.);
#3613=ORIENTED_EDGE('',*,*,#2650,.F.);
#3614=ORIENTED_EDGE('',*,*,#2649,.T.);
#3615=ORIENTED_EDGE('',*,*,#2651,.F.);
#3616=ORIENTED_EDGE('',*,*,#2651,.T.);
#3617=ORIENTED_EDGE('',*,*,#2652,.T.);
#3618=ORIENTED_EDGE('',*,*,#2648,.F.);
#3619=ORIENTED_EDGE('',*,*,#2652,.F.);
#3620=ORIENTED_EDGE('',*,*,#2653,.F.);
#3621=ORIENTED_EDGE('',*,*,#2654,.T.);
#3622=ORIENTED_EDGE('',*,*,#2655,.F.);
#3623=ORIENTED_EDGE('',*,*,#2656,.T.);
#3624=ORIENTED_EDGE('',*,*,#2653,.T.);
#3625=ORIENTED_EDGE('',*,*,#2656,.F.);
#3626=ORIENTED_EDGE('',*,*,#2655,.T.);
#3627=ORIENTED_EDGE('',*,*,#2657,.F.);
#3628=ORIENTED_EDGE('',*,*,#2657,.T.);
#3629=ORIENTED_EDGE('',*,*,#2658,.T.);
#3630=ORIENTED_EDGE('',*,*,#2654,.F.);
#3631=ORIENTED_EDGE('',*,*,#2658,.F.);
#3632=ORIENTED_EDGE('',*,*,#2659,.F.);
#3633=ORIENTED_EDGE('',*,*,#2660,.T.);
#3634=ORIENTED_EDGE('',*,*,#2661,.T.);
#3635=ORIENTED_EDGE('',*,*,#2660,.F.);
#3636=ORIENTED_EDGE('',*,*,#2662,.F.);
#3637=ORIENTED_EDGE('',*,*,#2663,.T.);
#3638=ORIENTED_EDGE('',*,*,#2664,.T.);
#3639=ORIENTED_EDGE('',*,*,#2663,.F.);
#3640=ORIENTED_EDGE('',*,*,#2662,.T.);
#3641=ORIENTED_EDGE('',*,*,#2659,.T.);
#3642=ORIENTED_EDGE('',*,*,#2664,.F.);
#3643=ORIENTED_EDGE('',*,*,#2661,.F.);
#3644=ORIENTED_EDGE('',*,*,#2665,.F.);
#3645=ORIENTED_EDGE('',*,*,#2666,.T.);
#3646=ORIENTED_EDGE('',*,*,#2667,.T.);
#3647=ORIENTED_EDGE('',*,*,#2666,.F.);
#3648=ORIENTED_EDGE('',*,*,#2668,.F.);
#3649=ORIENTED_EDGE('',*,*,#2669,.T.);
#3650=ORIENTED_EDGE('',*,*,#2670,.T.);
#3651=ORIENTED_EDGE('',*,*,#2669,.F.);
#3652=ORIENTED_EDGE('',*,*,#2668,.T.);
#3653=ORIENTED_EDGE('',*,*,#2665,.T.);
#3654=ORIENTED_EDGE('',*,*,#2670,.F.);
#3655=ORIENTED_EDGE('',*,*,#2667,.F.);
#3656=ORIENTED_EDGE('',*,*,#2671,.F.);
#3657=ORIENTED_EDGE('',*,*,#2672,.T.);
#3658=ORIENTED_EDGE('',*,*,#2673,.T.);
#3659=ORIENTED_EDGE('',*,*,#2672,.F.);
#3660=ORIENTED_EDGE('',*,*,#2674,.F.);
#3661=ORIENTED_EDGE('',*,*,#2675,.T.);
#3662=ORIENTED_EDGE('',*,*,#2676,.T.);
#3663=ORIENTED_EDGE('',*,*,#2675,.F.);
#3664=ORIENTED_EDGE('',*,*,#2674,.T.);
#3665=ORIENTED_EDGE('',*,*,#2671,.T.);
#3666=ORIENTED_EDGE('',*,*,#2676,.F.);
#3667=ORIENTED_EDGE('',*,*,#2673,.F.);
#3668=ORIENTED_EDGE('',*,*,#2677,.F.);
#3669=ORIENTED_EDGE('',*,*,#2678,.T.);
#3670=ORIENTED_EDGE('',*,*,#2679,.T.);
#3671=ORIENTED_EDGE('',*,*,#2678,.F.);
#3672=ORIENTED_EDGE('',*,*,#2680,.F.);
#3673=ORIENTED_EDGE('',*,*,#2681,.T.);
#3674=ORIENTED_EDGE('',*,*,#2682,.T.);
#3675=ORIENTED_EDGE('',*,*,#2681,.F.);
#3676=ORIENTED_EDGE('',*,*,#2680,.T.);
#3677=ORIENTED_EDGE('',*,*,#2677,.T.);
#3678=ORIENTED_EDGE('',*,*,#2682,.F.);
#3679=ORIENTED_EDGE('',*,*,#2679,.F.);
#3680=ORIENTED_EDGE('',*,*,#2683,.F.);
#3681=ORIENTED_EDGE('',*,*,#2684,.T.);
#3682=ORIENTED_EDGE('',*,*,#2685,.F.);
#3683=ORIENTED_EDGE('',*,*,#2684,.F.);
#3684=ORIENTED_EDGE('',*,*,#2686,.F.);
#3685=ORIENTED_EDGE('',*,*,#2687,.T.);
#3686=ORIENTED_EDGE('',*,*,#2688,.F.);
#3687=ORIENTED_EDGE('',*,*,#2687,.F.);
#3688=ORIENTED_EDGE('',*,*,#2689,.F.);
#3689=ORIENTED_EDGE('',*,*,#2690,.T.);
#3690=ORIENTED_EDGE('',*,*,#2691,.F.);
#3691=ORIENTED_EDGE('',*,*,#2690,.F.);
#3692=ORIENTED_EDGE('',*,*,#2692,.F.);
#3693=ORIENTED_EDGE('',*,*,#2693,.T.);
#3694=ORIENTED_EDGE('',*,*,#2694,.F.);
#3695=ORIENTED_EDGE('',*,*,#2693,.F.);
#3696=ORIENTED_EDGE('',*,*,#2695,.F.);
#3697=ORIENTED_EDGE('',*,*,#2696,.T.);
#3698=ORIENTED_EDGE('',*,*,#2697,.T.);
#3699=ORIENTED_EDGE('',*,*,#2696,.F.);
#3700=ORIENTED_EDGE('',*,*,#2698,.F.);
#3701=ORIENTED_EDGE('',*,*,#2697,.F.);
#3702=ORIENTED_EDGE('',*,*,#2698,.T.);
#3703=ORIENTED_EDGE('',*,*,#2699,.T.);
#3704=ORIENTED_EDGE('',*,*,#2700,.T.);
#3705=ORIENTED_EDGE('',*,*,#2699,.F.);
#3706=ORIENTED_EDGE('',*,*,#2701,.F.);
#3707=ORIENTED_EDGE('',*,*,#2702,.T.);
#3708=ORIENTED_EDGE('',*,*,#2703,.T.);
#3709=ORIENTED_EDGE('',*,*,#2702,.F.);
#3710=ORIENTED_EDGE('',*,*,#2701,.T.);
#3711=ORIENTED_EDGE('',*,*,#2695,.T.);
#3712=ORIENTED_EDGE('',*,*,#2694,.T.);
#3713=ORIENTED_EDGE('',*,*,#2691,.T.);
#3714=ORIENTED_EDGE('',*,*,#2688,.T.);
#3715=ORIENTED_EDGE('',*,*,#2685,.T.);
#3716=ORIENTED_EDGE('',*,*,#2703,.F.);
#3717=ORIENTED_EDGE('',*,*,#2700,.F.);
#3718=ORIENTED_EDGE('',*,*,#2692,.T.);
#3719=ORIENTED_EDGE('',*,*,#2689,.T.);
#3720=ORIENTED_EDGE('',*,*,#2686,.T.);
#3721=ORIENTED_EDGE('',*,*,#2683,.T.);
#3722=ORIENTED_EDGE('',*,*,#2704,.F.);
#3723=ORIENTED_EDGE('',*,*,#2705,.T.);
#3724=ORIENTED_EDGE('',*,*,#2706,.F.);
#3725=ORIENTED_EDGE('',*,*,#2705,.F.);
#3726=ORIENTED_EDGE('',*,*,#2707,.F.);
#3727=ORIENTED_EDGE('',*,*,#2708,.T.);
#3728=ORIENTED_EDGE('',*,*,#2709,.F.);
#3729=ORIENTED_EDGE('',*,*,#2708,.F.);
#3730=ORIENTED_EDGE('',*,*,#2710,.F.);
#3731=ORIENTED_EDGE('',*,*,#2711,.T.);
#3732=ORIENTED_EDGE('',*,*,#2712,.F.);
#3733=ORIENTED_EDGE('',*,*,#2711,.F.);
#3734=ORIENTED_EDGE('',*,*,#2713,.F.);
#3735=ORIENTED_EDGE('',*,*,#2714,.T.);
#3736=ORIENTED_EDGE('',*,*,#2715,.F.);
#3737=ORIENTED_EDGE('',*,*,#2714,.F.);
#3738=ORIENTED_EDGE('',*,*,#2716,.F.);
#3739=ORIENTED_EDGE('',*,*,#2717,.T.);
#3740=ORIENTED_EDGE('',*,*,#2718,.T.);
#3741=ORIENTED_EDGE('',*,*,#2717,.F.);
#3742=ORIENTED_EDGE('',*,*,#2719,.F.);
#3743=ORIENTED_EDGE('',*,*,#2720,.T.);
#3744=ORIENTED_EDGE('',*,*,#2721,.T.);
#3745=ORIENTED_EDGE('',*,*,#2720,.F.);
#3746=ORIENTED_EDGE('',*,*,#2719,.T.);
#3747=ORIENTED_EDGE('',*,*,#2716,.T.);
#3748=ORIENTED_EDGE('',*,*,#2715,.T.);
#3749=ORIENTED_EDGE('',*,*,#2712,.T.);
#3750=ORIENTED_EDGE('',*,*,#2709,.T.);
#3751=ORIENTED_EDGE('',*,*,#2706,.T.);
#3752=ORIENTED_EDGE('',*,*,#2721,.F.);
#3753=ORIENTED_EDGE('',*,*,#2718,.F.);
#3754=ORIENTED_EDGE('',*,*,#2713,.T.);
#3755=ORIENTED_EDGE('',*,*,#2710,.T.);
#3756=ORIENTED_EDGE('',*,*,#2707,.T.);
#3757=ORIENTED_EDGE('',*,*,#2704,.T.);
#3758=ORIENTED_EDGE('',*,*,#2722,.F.);
#3759=ORIENTED_EDGE('',*,*,#2723,.F.);
#3760=ORIENTED_EDGE('',*,*,#2724,.T.);
#3761=ORIENTED_EDGE('',*,*,#2722,.T.);
#3762=ORIENTED_EDGE('',*,*,#2724,.F.);
#3763=ORIENTED_EDGE('',*,*,#2725,.F.);
#3764=ORIENTED_EDGE('',*,*,#2726,.T.);
#3765=ORIENTED_EDGE('',*,*,#2723,.T.);
#3766=ORIENTED_EDGE('',*,*,#2726,.F.);
#3767=ORIENTED_EDGE('',*,*,#2727,.F.);
#3768=ORIENTED_EDGE('',*,*,#2728,.T.);
#3769=ORIENTED_EDGE('',*,*,#2725,.T.);
#3770=ORIENTED_EDGE('',*,*,#2728,.F.);
#3771=ORIENTED_EDGE('',*,*,#2727,.T.);
#3772=ORIENTED_EDGE('',*,*,#2729,.F.);
#3773=ORIENTED_EDGE('',*,*,#2730,.F.);
#3774=ORIENTED_EDGE('',*,*,#2731,.T.);
#3775=ORIENTED_EDGE('',*,*,#2729,.T.);
#3776=ORIENTED_EDGE('',*,*,#2731,.F.);
#3777=ORIENTED_EDGE('',*,*,#2732,.F.);
#3778=ORIENTED_EDGE('',*,*,#2733,.T.);
#3779=ORIENTED_EDGE('',*,*,#2730,.T.);
#3780=ORIENTED_EDGE('',*,*,#2733,.F.);
#3781=ORIENTED_EDGE('',*,*,#2734,.F.);
#3782=ORIENTED_EDGE('',*,*,#2735,.T.);
#3783=ORIENTED_EDGE('',*,*,#2732,.T.);
#3784=ORIENTED_EDGE('',*,*,#2735,.F.);
#3785=ORIENTED_EDGE('',*,*,#2734,.T.);
#3786=ORIENTED_EDGE('',*,*,#2736,.T.);
#3787=ORIENTED_EDGE('',*,*,#2737,.T.);
#3788=ORIENTED_EDGE('',*,*,#2738,.T.);
#3789=ORIENTED_EDGE('',*,*,#2739,.F.);
#3790=ORIENTED_EDGE('',*,*,#2740,.T.);
#3791=ORIENTED_EDGE('',*,*,#2741,.T.);
#3792=ORIENTED_EDGE('',*,*,#2742,.T.);
#3793=ORIENTED_EDGE('',*,*,#2737,.F.);
#3794=ORIENTED_EDGE('',*,*,#2743,.T.);
#3795=ORIENTED_EDGE('',*,*,#2744,.T.);
#3796=ORIENTED_EDGE('',*,*,#2745,.T.);
#3797=ORIENTED_EDGE('',*,*,#2741,.F.);
#3798=ORIENTED_EDGE('',*,*,#2746,.T.);
#3799=ORIENTED_EDGE('',*,*,#2747,.T.);
#3800=ORIENTED_EDGE('',*,*,#2748,.T.);
#3801=ORIENTED_EDGE('',*,*,#2744,.F.);
#3802=ORIENTED_EDGE('',*,*,#2749,.T.);
#3803=ORIENTED_EDGE('',*,*,#2750,.T.);
#3804=ORIENTED_EDGE('',*,*,#2751,.T.);
#3805=ORIENTED_EDGE('',*,*,#2747,.F.);
#3806=ORIENTED_EDGE('',*,*,#2752,.T.);
#3807=ORIENTED_EDGE('',*,*,#2739,.T.);
#3808=ORIENTED_EDGE('',*,*,#2753,.T.);
#3809=ORIENTED_EDGE('',*,*,#2750,.F.);
#3810=ORIENTED_EDGE('',*,*,#2752,.F.);
#3811=ORIENTED_EDGE('',*,*,#2749,.F.);
#3812=ORIENTED_EDGE('',*,*,#2746,.F.);
#3813=ORIENTED_EDGE('',*,*,#2743,.F.);
#3814=ORIENTED_EDGE('',*,*,#2740,.F.);
#3815=ORIENTED_EDGE('',*,*,#2736,.F.);
#3816=ORIENTED_EDGE('',*,*,#2753,.F.);
#3817=ORIENTED_EDGE('',*,*,#2738,.F.);
#3818=ORIENTED_EDGE('',*,*,#2742,.F.);
#3819=ORIENTED_EDGE('',*,*,#2745,.F.);
#3820=ORIENTED_EDGE('',*,*,#2748,.F.);
#3821=ORIENTED_EDGE('',*,*,#2751,.F.);
#3822=PLANE('',#4429);
#3823=PLANE('',#4430);
#3824=PLANE('',#4431);
#3825=PLANE('',#4432);
#3826=PLANE('',#4433);
#3827=PLANE('',#4434);
#3828=PLANE('',#4435);
#3829=PLANE('',#4436);
#3830=PLANE('',#4437);
#3831=PLANE('',#4438);
#3832=PLANE('',#4439);
#3833=PLANE('',#4440);
#3834=PLANE('',#4441);
#3835=PLANE('',#4442);
#3836=PLANE('',#4443);
#3837=PLANE('',#4444);
#3838=PLANE('',#4445);
#3839=PLANE('',#4446);
#3840=PLANE('',#4447);
#3841=PLANE('',#4448);
#3842=PLANE('',#4449);
#3843=PLANE('',#4450);
#3844=PLANE('',#4451);
#3845=PLANE('',#4452);
#3846=PLANE('',#4453);
#3847=PLANE('',#4454);
#3848=PLANE('',#4455);
#3849=PLANE('',#4456);
#3850=PLANE('',#4457);
#3851=PLANE('',#4458);
#3852=PLANE('',#4459);
#3853=PLANE('',#4460);
#3854=PLANE('',#4461);
#3855=PLANE('',#4462);
#3856=PLANE('',#4463);
#3857=PLANE('',#4464);
#3858=PLANE('',#4468);
#3859=PLANE('',#4469);
#3860=PLANE('',#4470);
#3861=PLANE('',#4471);
#3862=PLANE('',#4472);
#3863=PLANE('',#4473);
#3864=PLANE('',#4474);
#3865=PLANE('',#4475);
#3866=PLANE('',#4476);
#3867=PLANE('',#4477);
#3868=PLANE('',#4483);
#3869=PLANE('',#4487);
#3870=PLANE('',#4488);
#3871=PLANE('',#4491);
#3872=PLANE('',#4499);
#3873=PLANE('',#4500);
#3874=PLANE('',#4508);
#3875=PLANE('',#4516);
#3876=PLANE('',#4518);
#3877=PLANE('',#4520);
#3878=PLANE('',#4521);
#3879=PLANE('',#4522);
#3880=PLANE('',#4529);
#3881=PLANE('',#4530);
#3882=PLANE('',#4531);
#3883=PLANE('',#4532);
#3884=PLANE('',#4533);
#3885=PLANE('',#4534);
#3886=PLANE('',#4535);
#3887=PLANE('',#4536);
#3888=PLANE('',#4544);
#3889=PLANE('',#4552);
#3890=PLANE('',#4554);
#3891=PLANE('',#4556);
#3892=PLANE('',#4557);
#3893=PLANE('',#4558);
#3894=PLANE('',#4565);
#3895=PLANE('',#4566);
#3896=PLANE('',#4567);
#3897=PLANE('',#4568);
#3898=PLANE('',#4569);
#3899=PLANE('',#4570);
#3900=PLANE('',#4571);
#3901=PLANE('',#4572);
#3902=PLANE('',#4574);
#3903=PLANE('',#4575);
#3904=PLANE('',#4576);
#3905=PLANE('',#4577);
#3906=PLANE('',#4578);
#3907=PLANE('',#4579);
#3908=PLANE('',#4580);
#3909=PLANE('',#4581);
#3910=PLANE('',#4582);
#3911=PLANE('',#4584);
#3912=PLANE('',#4592);
#3913=PLANE('',#4598);
#3914=PLANE('',#4599);
#3915=PLANE('',#4600);
#3916=PLANE('',#4602);
#3917=PLANE('',#4603);
#3918=PLANE('',#4604);
#3919=PLANE('',#4605);
#3920=PLANE('',#4606);
#3921=PLANE('',#4607);
#3922=PLANE('',#4614);
#3923=PLANE('',#4615);
#3924=PLANE('',#4616);
#3925=PLANE('',#4617);
#3926=PLANE('',#4633);
#3927=PLANE('',#4636);
#3928=PLANE('',#4648);
#3929=PLANE('',#4657);
#3930=PLANE('',#4690);
#3931=PLANE('',#4695);
#3932=PLANE('',#4700);
#3933=PLANE('',#4705);
#3934=PLANE('',#4710);
#3935=PLANE('',#4715);
#3936=PLANE('',#4724);
#3937=PLANE('',#4728);
#3938=PLANE('',#4729);
#3939=PLANE('',#4731);
#3940=PLANE('',#4736);
#3941=PLANE('',#4739);
#3942=PLANE('',#4744);
#3943=PLANE('',#4759);
#3944=PLANE('',#4760);
#3945=PLANE('',#4768);
#3946=PLANE('',#4769);
#3947=PLANE('',#4777);
#3948=PLANE('',#4778);
#3949=PLANE('',#4787);
#3950=PLANE('',#4788);
#3951=PLANE('',#4805);
#3952=PLANE('',#4812);
#3953=PLANE('',#4813);
#3954=PLANE('',#4833);
#3955=PLANE('',#4834);
#3956=PLANE('',#4836);
#3957=PLANE('',#4844);
#3958=PLANE('',#4852);
#3959=PLANE('',#4853);
#3960=PLANE('',#4854);
#3961=PLANE('',#4855);
#3962=PLANE('',#4856);
#3963=PLANE('',#4857);
#3964=PLANE('',#4858);
#3965=PLANE('',#4859);
#3966=PLANE('',#4860);
#3967=ADVANCED_FACE('',(#652),#3822,.F.);
#3968=ADVANCED_FACE('',(#653),#3823,.F.);
#3969=ADVANCED_FACE('',(#654),#3824,.F.);
#3970=ADVANCED_FACE('',(#655),#3825,.F.);
#3971=ADVANCED_FACE('',(#656),#3826,.F.);
#3972=ADVANCED_FACE('',(#657),#3827,.F.);
#3973=ADVANCED_FACE('',(#658),#3828,.F.);
#3974=ADVANCED_FACE('',(#659),#3829,.F.);
#3975=ADVANCED_FACE('',(#660),#3830,.F.);
#3976=ADVANCED_FACE('',(#661),#3831,.F.);
#3977=ADVANCED_FACE('',(#662),#3832,.F.);
#3978=ADVANCED_FACE('',(#663),#3833,.F.);
#3979=ADVANCED_FACE('',(#664),#3834,.F.);
#3980=ADVANCED_FACE('',(#665),#3835,.F.);
#3981=ADVANCED_FACE('',(#666),#3836,.F.);
#3982=ADVANCED_FACE('',(#667),#3837,.F.);
#3983=ADVANCED_FACE('',(#668),#3838,.F.);
#3984=ADVANCED_FACE('',(#669),#3839,.F.);
#3985=ADVANCED_FACE('',(#670),#3840,.F.);
#3986=ADVANCED_FACE('',(#671),#3841,.F.);
#3987=ADVANCED_FACE('',(#672),#3842,.F.);
#3988=ADVANCED_FACE('',(#673),#3843,.F.);
#3989=ADVANCED_FACE('',(#674),#3844,.F.);
#3990=ADVANCED_FACE('',(#675),#3845,.F.);
#3991=ADVANCED_FACE('',(#676),#3846,.F.);
#3992=ADVANCED_FACE('',(#677),#3847,.F.);
#3993=ADVANCED_FACE('',(#678),#3848,.F.);
#3994=ADVANCED_FACE('',(#679),#3849,.F.);
#3995=ADVANCED_FACE('',(#680),#3850,.F.);
#3996=ADVANCED_FACE('',(#681),#3851,.F.);
#3997=ADVANCED_FACE('',(#682),#3852,.F.);
#3998=ADVANCED_FACE('',(#683),#3853,.F.);
#3999=ADVANCED_FACE('',(#684),#3854,.F.);
#4000=ADVANCED_FACE('',(#685),#3855,.F.);
#4001=ADVANCED_FACE('',(#686),#3856,.F.);
#4002=ADVANCED_FACE('',(#687),#3857,.F.);
#4003=ADVANCED_FACE('',(#688),#594,.F.);
#4004=ADVANCED_FACE('',(#689),#3858,.T.);
#4005=ADVANCED_FACE('',(#690),#3859,.T.);
#4006=ADVANCED_FACE('',(#691),#3860,.T.);
#4007=ADVANCED_FACE('',(#692),#3861,.T.);
#4008=ADVANCED_FACE('',(#693),#3862,.T.);
#4009=ADVANCED_FACE('',(#694),#3863,.T.);
#4010=ADVANCED_FACE('',(#695),#3864,.T.);
#4011=ADVANCED_FACE('',(#696),#3865,.T.);
#4012=ADVANCED_FACE('',(#697,#362),#3866,.T.);
#4013=ADVANCED_FACE('',(#698,#363),#3867,.F.);
#4014=ADVANCED_FACE('',(#699),#595,.F.);
#4015=ADVANCED_FACE('',(#700),#3868,.T.);
#4016=ADVANCED_FACE('',(#701),#596,.F.);
#4017=ADVANCED_FACE('',(#702),#3869,.F.);
#4018=ADVANCED_FACE('',(#703,#364),#3870,.T.);
#4019=ADVANCED_FACE('',(#704,#365),#3871,.F.);
#4020=ADVANCED_FACE('',(#705),#597,.T.);
#4021=ADVANCED_FACE('',(#706),#598,.T.);
#4022=ADVANCED_FACE('',(#707),#599,.T.);
#4023=ADVANCED_FACE('',(#708,#366),#3872,.T.);
#4024=ADVANCED_FACE('',(#709,#367),#3873,.F.);
#4025=ADVANCED_FACE('',(#710),#600,.F.);
#4026=ADVANCED_FACE('',(#711),#601,.F.);
#4027=ADVANCED_FACE('',(#712,#368),#3874,.T.);
#4028=ADVANCED_FACE('',(#713),#602,.F.);
#4029=ADVANCED_FACE('',(#714),#603,.F.);
#4030=ADVANCED_FACE('',(#715,#369),#3875,.T.);
#4031=ADVANCED_FACE('',(#716,#370),#3876,.T.);
#4032=ADVANCED_FACE('',(#717),#3877,.T.);
#4033=ADVANCED_FACE('',(#718),#3878,.T.);
#4034=ADVANCED_FACE('',(#719),#3879,.T.);
#4035=ADVANCED_FACE('',(#720),#604,.F.);
#4036=ADVANCED_FACE('',(#721),#605,.F.);
#4037=ADVANCED_FACE('',(#722),#606,.F.);
#4038=ADVANCED_FACE('',(#723),#3880,.T.);
#4039=ADVANCED_FACE('',(#724),#3881,.T.);
#4040=ADVANCED_FACE('',(#725),#3882,.T.);
#4041=ADVANCED_FACE('',(#726),#3883,.F.);
#4042=ADVANCED_FACE('',(#727,#371),#3884,.T.);
#4043=ADVANCED_FACE('',(#728),#3885,.T.);
#4044=ADVANCED_FACE('',(#729),#3886,.T.);
#4045=ADVANCED_FACE('',(#730,#372,#373),#3887,.F.);
#4046=ADVANCED_FACE('',(#731),#607,.F.);
#4047=ADVANCED_FACE('',(#732),#608,.F.);
#4048=ADVANCED_FACE('',(#733,#374),#3888,.T.);
#4049=ADVANCED_FACE('',(#734),#609,.F.);
#4050=ADVANCED_FACE('',(#735),#610,.F.);
#4051=ADVANCED_FACE('',(#736,#375),#3889,.T.);
#4052=ADVANCED_FACE('',(#737,#376),#3890,.T.);
#4053=ADVANCED_FACE('',(#738),#3891,.T.);
#4054=ADVANCED_FACE('',(#739),#3892,.T.);
#4055=ADVANCED_FACE('',(#740),#3893,.T.);
#4056=ADVANCED_FACE('',(#741),#611,.F.);
#4057=ADVANCED_FACE('',(#742),#612,.F.);
#4058=ADVANCED_FACE('',(#743),#613,.F.);
#4059=ADVANCED_FACE('',(#744),#3894,.T.);
#4060=ADVANCED_FACE('',(#745),#3895,.T.);
#4061=ADVANCED_FACE('',(#746),#3896,.T.);
#4062=ADVANCED_FACE('',(#747),#3897,.F.);
#4063=ADVANCED_FACE('',(#748,#377),#3898,.T.);
#4064=ADVANCED_FACE('',(#749),#3899,.T.);
#4065=ADVANCED_FACE('',(#750),#3900,.T.);
#4066=ADVANCED_FACE('',(#751,#378,#379),#3901,.F.);
#4067=ADVANCED_FACE('',(#752),#3902,.F.);
#4068=ADVANCED_FACE('',(#753),#3903,.F.);
#4069=ADVANCED_FACE('',(#754),#3904,.F.);
#4070=ADVANCED_FACE('',(#755),#3905,.F.);
#4071=ADVANCED_FACE('',(#756),#3906,.F.);
#4072=ADVANCED_FACE('',(#757),#3907,.F.);
#4073=ADVANCED_FACE('',(#758),#3908,.F.);
#4074=ADVANCED_FACE('',(#759),#3909,.F.);
#4075=ADVANCED_FACE('',(#760),#3910,.F.);
#4076=ADVANCED_FACE('',(#761),#3911,.T.);
#4077=ADVANCED_FACE('',(#762),#261,.T.);
#4078=ADVANCED_FACE('',(#763),#614,.T.);
#4079=ADVANCED_FACE('',(#764),#262,.T.);
#4080=ADVANCED_FACE('',(#765,#380),#3912,.T.);
#4081=ADVANCED_FACE('',(#766),#263,.T.);
#4082=ADVANCED_FACE('',(#767),#615,.T.);
#4083=ADVANCED_FACE('',(#768),#3913,.F.);
#4084=ADVANCED_FACE('',(#769),#3914,.T.);
#4085=ADVANCED_FACE('',(#770,#381),#3915,.T.);
#4086=ADVANCED_FACE('',(#771),#3916,.T.);
#4087=ADVANCED_FACE('',(#772),#3917,.T.);
#4088=ADVANCED_FACE('',(#773),#3918,.F.);
#4089=ADVANCED_FACE('',(#774),#3919,.T.);
#4090=ADVANCED_FACE('',(#775),#3920,.T.);
#4091=ADVANCED_FACE('',(#776),#3921,.T.);
#4092=ADVANCED_FACE('',(#777),#616,.F.);
#4093=ADVANCED_FACE('',(#778),#3922,.F.);
#4094=ADVANCED_FACE('',(#779),#3923,.F.);
#4095=ADVANCED_FACE('',(#780),#3924,.T.);
#4096=ADVANCED_FACE('',(#781),#3925,.T.);
#4097=ADVANCED_FACE('',(#782),#257,.F.);
#4098=ADVANCED_FACE('',(#783),#617,.T.);
#4099=ADVANCED_FACE('',(#784),#618,.F.);
#4100=ADVANCED_FACE('',(#785),#264,.F.);
#4101=ADVANCED_FACE('',(#786,#382),#3926,.T.);
#4102=ADVANCED_FACE('',(#787),#619,.T.);
#4103=ADVANCED_FACE('',(#788,#383),#3927,.T.);
#4104=ADVANCED_FACE('',(#789),#265,.F.);
#4105=ADVANCED_FACE('',(#790),#258,.F.);
#4106=ADVANCED_FACE('',(#791),#620,.F.);
#4107=ADVANCED_FACE('',(#792,#384),#3928,.T.);
#4108=ADVANCED_FACE('',(#793),#266,.T.);
#4109=ADVANCED_FACE('',(#794),#621,.T.);
#4110=ADVANCED_FACE('',(#795),#267,.T.);
#4111=ADVANCED_FACE('',(#796,#385),#3929,.T.);
#4112=ADVANCED_FACE('',(#797),#622,.F.);
#4113=ADVANCED_FACE('',(#798),#241,.T.);
#4114=ADVANCED_FACE('',(#799),#242,.T.);
#4115=ADVANCED_FACE('',(#800),#243,.T.);
#4116=ADVANCED_FACE('',(#801),#244,.T.);
#4117=ADVANCED_FACE('',(#802),#245,.T.);
#4118=ADVANCED_FACE('',(#803),#246,.T.);
#4119=ADVANCED_FACE('',(#804),#247,.T.);
#4120=ADVANCED_FACE('',(#805),#248,.T.);
#4121=ADVANCED_FACE('',(#806),#249,.F.);
#4122=ADVANCED_FACE('',(#807),#623,.T.);
#4123=ADVANCED_FACE('',(#808),#3930,.T.);
#4124=ADVANCED_FACE('',(#809),#250,.F.);
#4125=ADVANCED_FACE('',(#810),#3931,.T.);
#4126=ADVANCED_FACE('',(#811),#251,.F.);
#4127=ADVANCED_FACE('',(#812),#3932,.T.);
#4128=ADVANCED_FACE('',(#813),#252,.F.);
#4129=ADVANCED_FACE('',(#814),#3933,.T.);
#4130=ADVANCED_FACE('',(#815),#253,.F.);
#4131=ADVANCED_FACE('',(#816),#3934,.T.);
#4132=ADVANCED_FACE('',(#817),#254,.F.);
#4133=ADVANCED_FACE('',(#818),#3935,.T.);
#4134=ADVANCED_FACE('',(#819),#255,.F.);
#4135=ADVANCED_FACE('',(#820),#624,.F.);
#4136=ADVANCED_FACE('',(#821),#3936,.T.);
#4137=ADVANCED_FACE('',(#822),#256,.F.);
#4138=ADVANCED_FACE('',(#823,#386),#3937,.T.);
#4139=ADVANCED_FACE('',(#824),#3938,.T.);
#4140=ADVANCED_FACE('',(#825,#387),#3939,.T.);
#4141=ADVANCED_FACE('',(#826),#625,.T.);
#4142=ADVANCED_FACE('',(#827,#388),#3940,.T.);
#4143=ADVANCED_FACE('',(#828),#626,.F.);
#4144=ADVANCED_FACE('',(#829,#389),#3941,.T.);
#4145=ADVANCED_FACE('',(#830),#627,.T.);
#4146=ADVANCED_FACE('',(#831,#390),#3942,.T.);
#4147=ADVANCED_FACE('',(#832),#628,.F.);
#4148=ADVANCED_FACE('',(#833),#629,.F.);
#4149=ADVANCED_FACE('',(#834),#630,.T.);
#4150=ADVANCED_FACE('',(#835,#391),#3943,.T.);
#4151=ADVANCED_FACE('',(#836,#392),#3944,.F.);
#4152=ADVANCED_FACE('',(#837),#631,.F.);
#4153=ADVANCED_FACE('',(#838),#632,.T.);
#4154=ADVANCED_FACE('',(#839,#393),#3945,.T.);
#4155=ADVANCED_FACE('',(#840,#394),#3946,.F.);
#4156=ADVANCED_FACE('',(#841),#633,.F.);
#4157=ADVANCED_FACE('',(#842),#634,.T.);
#4158=ADVANCED_FACE('',(#843,#395),#3947,.T.);
#4159=ADVANCED_FACE('',(#844,#396),#3948,.F.);
#4160=ADVANCED_FACE('',(#845),#635,.F.);
#4161=ADVANCED_FACE('',(#846),#636,.T.);
#4162=ADVANCED_FACE('',(#847,#397),#3949,.T.);
#4163=ADVANCED_FACE('',(#848,#398),#3950,.F.);
#4164=ADVANCED_FACE('',(#849),#637,.F.);
#4165=ADVANCED_FACE('',(#850),#638,.F.);
#4166=ADVANCED_FACE('',(#851),#639,.F.);
#4167=ADVANCED_FACE('',(#852),#640,.F.);
#4168=ADVANCED_FACE('',(#853),#641,.F.);
#4169=ADVANCED_FACE('',(#854,#399),#3951,.F.);
#4170=ADVANCED_FACE('',(#855),#642,.F.);
#4171=ADVANCED_FACE('',(#856),#643,.T.);
#4172=ADVANCED_FACE('',(#857,#400,#401,#402,#403,#404),#3952,.T.);
#4173=ADVANCED_FACE('',(#858,#405,#406,#407,#408,#409),#3953,.F.);
#4174=ADVANCED_FACE('',(#859),#644,.F.);
#4175=ADVANCED_FACE('',(#860),#645,.F.);
#4176=ADVANCED_FACE('',(#861),#646,.F.);
#4177=ADVANCED_FACE('',(#862),#647,.F.);
#4178=ADVANCED_FACE('',(#863),#648,.F.);
#4179=ADVANCED_FACE('',(#864),#649,.T.);
#4180=ADVANCED_FACE('',(#865,#410,#411,#412,#413,#414),#3954,.T.);
#4181=ADVANCED_FACE('',(#866,#415,#416,#417,#418,#419),#3955,.F.);
#4182=ADVANCED_FACE('',(#867),#3956,.T.);
#4183=ADVANCED_FACE('',(#868),#268,.T.);
#4184=ADVANCED_FACE('',(#869),#650,.T.);
#4185=ADVANCED_FACE('',(#870),#269,.T.);
#4186=ADVANCED_FACE('',(#871,#420),#3957,.T.);
#4187=ADVANCED_FACE('',(#872),#270,.T.);
#4188=ADVANCED_FACE('',(#873),#651,.T.);
#4189=ADVANCED_FACE('',(#874),#271,.T.);
#4190=ADVANCED_FACE('',(#875),#3958,.T.);
#4191=ADVANCED_FACE('',(#876),#3959,.F.);
#4192=ADVANCED_FACE('',(#877),#3960,.F.);
#4193=ADVANCED_FACE('',(#878),#3961,.F.);
#4194=ADVANCED_FACE('',(#879),#3962,.F.);
#4195=ADVANCED_FACE('',(#880),#3963,.F.);
#4196=ADVANCED_FACE('',(#881),#3964,.F.);
#4197=ADVANCED_FACE('',(#882),#3965,.F.);
#4198=ADVANCED_FACE('',(#883),#3966,.F.);
#4199=CLOSED_SHELL('',(#3967,#3968,#3969,#3970,#3971,#3972,#3973,#3974,
#3975,#3976,#3977,#3978,#3979,#3980,#3981,#3982,#3983,#3984,#3985,#3986,
#3987,#3988,#3989,#3990,#3991,#3992,#3993,#3994,#3995,#3996,#3997,#3998,
#3999,#4000,#4001,#4002,#4003,#4004,#4005,#4006,#4007,#4008,#4009,#4010,
#4011,#4012,#4013));
#4200=CLOSED_SHELL('',(#4014,#4015,#4016,#4017,#4018,#4019,#4020,#4021,
#4022,#4023,#4024));
#4201=CLOSED_SHELL('',(#4025,#4026,#4027,#4028,#4029,#4030,#4031,#4032,
#4033,#4034,#4035,#4036,#4037,#4038,#4039,#4040,#4041,#4042,#4043,#4044,
#4045));
#4202=CLOSED_SHELL('',(#4046,#4047,#4048,#4049,#4050,#4051,#4052,#4053,
#4054,#4055,#4056,#4057,#4058,#4059,#4060,#4061,#4062,#4063,#4064,#4065,
#4066));
#4203=CLOSED_SHELL('',(#4067,#4068,#4069,#4070,#4071,#4072,#4073,#4074));
#4204=CLOSED_SHELL('',(#4075,#4076,#4077,#4078,#4079,#4080,#4081,#4082));
#4205=CLOSED_SHELL('',(#4083,#4084,#4085,#4086,#4087,#4088,#4089,#4090,
#4091,#4092,#4093,#4094,#4095,#4096));
#4206=CLOSED_SHELL('',(#4097,#4098,#4099,#4100,#4101,#4102,#4103,#4104));
#4207=CLOSED_SHELL('',(#4105,#4106,#4107,#4108,#4109,#4110,#4111,#4112));
#4208=CLOSED_SHELL('',(#4113));
#4209=CLOSED_SHELL('',(#4114));
#4210=CLOSED_SHELL('',(#4115));
#4211=CLOSED_SHELL('',(#4116));
#4212=CLOSED_SHELL('',(#4117));
#4213=CLOSED_SHELL('',(#4118));
#4214=CLOSED_SHELL('',(#4119));
#4215=CLOSED_SHELL('',(#4120));
#4216=CLOSED_SHELL('',(#4121,#4122,#4123,#4124,#4125,#4126,#4127,#4128,
#4129,#4130,#4131,#4132,#4133,#4134,#4135,#4136,#4137,#4138,#4139));
#4217=CLOSED_SHELL('',(#4140,#4141,#4142,#4143));
#4218=CLOSED_SHELL('',(#4144,#4145,#4146,#4147));
#4219=CLOSED_SHELL('',(#4148,#4149,#4150,#4151));
#4220=CLOSED_SHELL('',(#4152,#4153,#4154,#4155));
#4221=CLOSED_SHELL('',(#4156,#4157,#4158,#4159));
#4222=CLOSED_SHELL('',(#4160,#4161,#4162,#4163));
#4223=CLOSED_SHELL('',(#4164,#4165,#4166,#4167,#4168,#4169,#4170,#4171,
#4172,#4173));
#4224=CLOSED_SHELL('',(#4174,#4175,#4176,#4177,#4178,#4179,#4180,#4181));
#4225=CLOSED_SHELL('',(#4182,#4183,#4184,#4185,#4186,#4187,#4188,#4189,
#4190));
#4226=CLOSED_SHELL('',(#4191,#4192,#4193,#4194,#4195,#4196,#4197,#4198));
#4227=DERIVED_UNIT_ELEMENT(#4263,1.);
#4228=DERIVED_UNIT_ELEMENT(#7808,-3.);
#4229=DERIVED_UNIT_ELEMENT(#4263,1.);
#4230=DERIVED_UNIT_ELEMENT(#7808,-3.);
#4231=DERIVED_UNIT_ELEMENT(#4263,1.);
#4232=DERIVED_UNIT_ELEMENT(#7808,-3.);
#4233=DERIVED_UNIT_ELEMENT(#4263,1.);
#4234=DERIVED_UNIT_ELEMENT(#7808,-3.);
#4235=DERIVED_UNIT_ELEMENT(#4263,1.);
#4236=DERIVED_UNIT_ELEMENT(#7808,-3.);
#4237=DERIVED_UNIT_ELEMENT(#4263,1.);
#4238=DERIVED_UNIT_ELEMENT(#7808,-3.);
#4239=DERIVED_UNIT_ELEMENT(#4263,1.);
#4240=DERIVED_UNIT_ELEMENT(#7808,-3.);
#4241=DERIVED_UNIT_ELEMENT(#4263,1.);
#4242=DERIVED_UNIT_ELEMENT(#7808,-3.);
#4243=DERIVED_UNIT_ELEMENT(#4263,1.);
#4244=DERIVED_UNIT_ELEMENT(#7808,-3.);
#4245=DERIVED_UNIT_ELEMENT(#4263,1.);
#4246=DERIVED_UNIT_ELEMENT(#7808,-3.);
#4247=DERIVED_UNIT_ELEMENT(#4263,1.);
#4248=DERIVED_UNIT_ELEMENT(#7808,-3.);
#4249=DERIVED_UNIT_ELEMENT(#4263,1.);
#4250=DERIVED_UNIT_ELEMENT(#7808,-3.);
#4251=DERIVED_UNIT_ELEMENT(#4263,1.);
#4252=DERIVED_UNIT_ELEMENT(#7808,-3.);
#4253=DERIVED_UNIT_ELEMENT(#4263,1.);
#4254=DERIVED_UNIT_ELEMENT(#7808,-3.);
#4255=DERIVED_UNIT_ELEMENT(#4263,1.);
#4256=DERIVED_UNIT_ELEMENT(#7808,-3.);
#4257=DERIVED_UNIT_ELEMENT(#4263,1.);
#4258=DERIVED_UNIT_ELEMENT(#7808,-3.);
#4259=DERIVED_UNIT_ELEMENT(#4263,1.);
#4260=DERIVED_UNIT_ELEMENT(#7808,-3.);
#4261=DERIVED_UNIT_ELEMENT(#4263,1.);
#4262=DERIVED_UNIT_ELEMENT(#7808,-3.);
#4263=(
MASS_UNIT()
NAMED_UNIT(*)
SI_UNIT(.KILO.,.GRAM.)
);
#4264=DERIVED_UNIT((#4227,#4228));
#4265=DERIVED_UNIT((#4229,#4230));
#4266=DERIVED_UNIT((#4231,#4232));
#4267=DERIVED_UNIT((#4233,#4234));
#4268=DERIVED_UNIT((#4235,#4236));
#4269=DERIVED_UNIT((#4237,#4238));
#4270=DERIVED_UNIT((#4239,#4240));
#4271=DERIVED_UNIT((#4241,#4242));
#4272=DERIVED_UNIT((#4243,#4244));
#4273=DERIVED_UNIT((#4245,#4246));
#4274=DERIVED_UNIT((#4247,#4248));
#4275=DERIVED_UNIT((#4249,#4250));
#4276=DERIVED_UNIT((#4251,#4252));
#4277=DERIVED_UNIT((#4253,#4254));
#4278=DERIVED_UNIT((#4255,#4256));
#4279=DERIVED_UNIT((#4257,#4258));
#4280=DERIVED_UNIT((#4259,#4260));
#4281=DERIVED_UNIT((#4261,#4262));
#4282=MEASURE_REPRESENTATION_ITEM('density measure',
POSITIVE_RATIO_MEASURE(7850.),#4264);
#4283=MEASURE_REPRESENTATION_ITEM('density measure',
POSITIVE_RATIO_MEASURE(7850.),#4265);
#4284=MEASURE_REPRESENTATION_ITEM('density measure',
POSITIVE_RATIO_MEASURE(7850.),#4266);
#4285=MEASURE_REPRESENTATION_ITEM('density measure',
POSITIVE_RATIO_MEASURE(7850.),#4267);
#4286=MEASURE_REPRESENTATION_ITEM('density measure',
POSITIVE_RATIO_MEASURE(7850.),#4268);
#4287=MEASURE_REPRESENTATION_ITEM('density measure',
POSITIVE_RATIO_MEASURE(7850.),#4269);
#4288=MEASURE_REPRESENTATION_ITEM('density measure',
POSITIVE_RATIO_MEASURE(7850.),#4270);
#4289=MEASURE_REPRESENTATION_ITEM('density measure',
POSITIVE_RATIO_MEASURE(7850.),#4271);
#4290=MEASURE_REPRESENTATION_ITEM('density measure',
POSITIVE_RATIO_MEASURE(7850.),#4272);
#4291=MEASURE_REPRESENTATION_ITEM('density measure',
POSITIVE_RATIO_MEASURE(7850.),#4273);
#4292=MEASURE_REPRESENTATION_ITEM('density measure',
POSITIVE_RATIO_MEASURE(7850.),#4274);
#4293=MEASURE_REPRESENTATION_ITEM('density measure',
POSITIVE_RATIO_MEASURE(7850.),#4275);
#4294=MEASURE_REPRESENTATION_ITEM('density measure',
POSITIVE_RATIO_MEASURE(7850.),#4276);
#4295=MEASURE_REPRESENTATION_ITEM('density measure',
POSITIVE_RATIO_MEASURE(7850.),#4277);
#4296=MEASURE_REPRESENTATION_ITEM('density measure',
POSITIVE_RATIO_MEASURE(7850.),#4278);
#4297=MEASURE_REPRESENTATION_ITEM('density measure',
POSITIVE_RATIO_MEASURE(7850.),#4279);
#4298=MEASURE_REPRESENTATION_ITEM('density measure',
POSITIVE_RATIO_MEASURE(7850.),#4280);
#4299=MEASURE_REPRESENTATION_ITEM('density measure',
POSITIVE_RATIO_MEASURE(7850.),#4281);
#4300=PROPERTY_DEFINITION_REPRESENTATION(#4390,#4336);
#4301=PROPERTY_DEFINITION_REPRESENTATION(#4391,#4337);
#4302=PROPERTY_DEFINITION_REPRESENTATION(#4392,#4338);
#4303=PROPERTY_DEFINITION_REPRESENTATION(#4393,#4339);
#4304=PROPERTY_DEFINITION_REPRESENTATION(#4394,#4340);
#4305=PROPERTY_DEFINITION_REPRESENTATION(#4395,#4341);
#4306=PROPERTY_DEFINITION_REPRESENTATION(#4396,#4342);
#4307=PROPERTY_DEFINITION_REPRESENTATION(#4397,#4343);
#4308=PROPERTY_DEFINITION_REPRESENTATION(#4398,#4344);
#4309=PROPERTY_DEFINITION_REPRESENTATION(#4399,#4345);
#4310=PROPERTY_DEFINITION_REPRESENTATION(#4400,#4346);
#4311=PROPERTY_DEFINITION_REPRESENTATION(#4401,#4347);
#4312=PROPERTY_DEFINITION_REPRESENTATION(#4402,#4348);
#4313=PROPERTY_DEFINITION_REPRESENTATION(#4403,#4349);
#4314=PROPERTY_DEFINITION_REPRESENTATION(#4404,#4350);
#4315=PROPERTY_DEFINITION_REPRESENTATION(#4405,#4351);
#4316=PROPERTY_DEFINITION_REPRESENTATION(#4406,#4352);
#4317=PROPERTY_DEFINITION_REPRESENTATION(#4407,#4353);
#4318=PROPERTY_DEFINITION_REPRESENTATION(#4408,#4354);
#4319=PROPERTY_DEFINITION_REPRESENTATION(#4409,#4355);
#4320=PROPERTY_DEFINITION_REPRESENTATION(#4410,#4356);
#4321=PROPERTY_DEFINITION_REPRESENTATION(#4411,#4357);
#4322=PROPERTY_DEFINITION_REPRESENTATION(#4412,#4358);
#4323=PROPERTY_DEFINITION_REPRESENTATION(#4413,#4359);
#4324=PROPERTY_DEFINITION_REPRESENTATION(#4414,#4360);
#4325=PROPERTY_DEFINITION_REPRESENTATION(#4415,#4361);
#4326=PROPERTY_DEFINITION_REPRESENTATION(#4416,#4362);
#4327=PROPERTY_DEFINITION_REPRESENTATION(#4417,#4363);
#4328=PROPERTY_DEFINITION_REPRESENTATION(#4418,#4364);
#4329=PROPERTY_DEFINITION_REPRESENTATION(#4419,#4365);
#4330=PROPERTY_DEFINITION_REPRESENTATION(#4420,#4366);
#4331=PROPERTY_DEFINITION_REPRESENTATION(#4421,#4367);
#4332=PROPERTY_DEFINITION_REPRESENTATION(#4422,#4368);
#4333=PROPERTY_DEFINITION_REPRESENTATION(#4423,#4369);
#4334=PROPERTY_DEFINITION_REPRESENTATION(#4424,#4370);
#4335=PROPERTY_DEFINITION_REPRESENTATION(#4425,#4371);
#4336=REPRESENTATION('material name',(#4372),#7785);
#4337=REPRESENTATION('density',(#4282),#7785);
#4338=REPRESENTATION('material name',(#4373),#7787);
#4339=REPRESENTATION('density',(#4283),#7787);
#4340=REPRESENTATION('material name',(#4374),#7788);
#4341=REPRESENTATION('density',(#4284),#7788);
#4342=REPRESENTATION('material name',(#4375),#7789);
#4343=REPRESENTATION('density',(#4285),#7789);
#4344=REPRESENTATION('material name',(#4376),#7790);
#4345=REPRESENTATION('density',(#4286),#7790);
#4346=REPRESENTATION('material name',(#4377),#7791);
#4347=REPRESENTATION('density',(#4287),#7791);
#4348=REPRESENTATION('material name',(#4378),#7793);
#4349=REPRESENTATION('density',(#4288),#7793);
#4350=REPRESENTATION('material name',(#4379),#7794);
#4351=REPRESENTATION('density',(#4289),#7794);
#4352=REPRESENTATION('material name',(#4380),#7795);
#4353=REPRESENTATION('density',(#4290),#7795);
#4354=REPRESENTATION('material name',(#4381),#7796);
#4355=REPRESENTATION('density',(#4291),#7796);
#4356=REPRESENTATION('material name',(#4382),#7797);
#4357=REPRESENTATION('density',(#4292),#7797);
#4358=REPRESENTATION('material name',(#4383),#7798);
#4359=REPRESENTATION('density',(#4293),#7798);
#4360=REPRESENTATION('material name',(#4384),#7799);
#4361=REPRESENTATION('density',(#4294),#7799);
#4362=REPRESENTATION('material name',(#4385),#7800);
#4363=REPRESENTATION('density',(#4295),#7800);
#4364=REPRESENTATION('material name',(#4386),#7802);
#4365=REPRESENTATION('density',(#4296),#7802);
#4366=REPRESENTATION('material name',(#4387),#7803);
#4367=REPRESENTATION('density',(#4297),#7803);
#4368=REPRESENTATION('material name',(#4388),#7804);
#4369=REPRESENTATION('density',(#4298),#7804);
#4370=REPRESENTATION('material name',(#4389),#7805);
#4371=REPRESENTATION('density',(#4299),#7805);
#4372=DESCRIPTIVE_REPRESENTATION_ITEM('Steel','Steel');
#4373=DESCRIPTIVE_REPRESENTATION_ITEM('Steel','Steel');
#4374=DESCRIPTIVE_REPRESENTATION_ITEM('Steel','Steel');
#4375=DESCRIPTIVE_REPRESENTATION_ITEM('Steel','Steel');
#4376=DESCRIPTIVE_REPRESENTATION_ITEM('Steel','Steel');
#4377=DESCRIPTIVE_REPRESENTATION_ITEM('Steel','Steel');
#4378=DESCRIPTIVE_REPRESENTATION_ITEM('Steel','Steel');
#4379=DESCRIPTIVE_REPRESENTATION_ITEM('Steel','Steel');
#4380=DESCRIPTIVE_REPRESENTATION_ITEM('Steel','Steel');
#4381=DESCRIPTIVE_REPRESENTATION_ITEM('Steel','Steel');
#4382=DESCRIPTIVE_REPRESENTATION_ITEM('Steel','Steel');
#4383=DESCRIPTIVE_REPRESENTATION_ITEM('Steel','Steel');
#4384=DESCRIPTIVE_REPRESENTATION_ITEM('Steel','Steel');
#4385=DESCRIPTIVE_REPRESENTATION_ITEM('Steel','Steel');
#4386=DESCRIPTIVE_REPRESENTATION_ITEM('Steel','Steel');
#4387=DESCRIPTIVE_REPRESENTATION_ITEM('Steel','Steel');
#4388=DESCRIPTIVE_REPRESENTATION_ITEM('Steel','Steel');
#4389=DESCRIPTIVE_REPRESENTATION_ITEM('Steel','Steel');
#4390=PROPERTY_DEFINITION('material property','material name',#7936);
#4391=PROPERTY_DEFINITION('material property','density of part',#7936);
#4392=PROPERTY_DEFINITION('material property','material name',#7938);
#4393=PROPERTY_DEFINITION('material property','density of part',#7938);
#4394=PROPERTY_DEFINITION('material property','material name',#7939);
#4395=PROPERTY_DEFINITION('material property','density of part',#7939);
#4396=PROPERTY_DEFINITION('material property','material name',#7940);
#4397=PROPERTY_DEFINITION('material property','density of part',#7940);
#4398=PROPERTY_DEFINITION('material property','material name',#7941);
#4399=PROPERTY_DEFINITION('material property','density of part',#7941);
#4400=PROPERTY_DEFINITION('material property','material name',#7942);
#4401=PROPERTY_DEFINITION('material property','density of part',#7942);
#4402=PROPERTY_DEFINITION('material property','material name',#7944);
#4403=PROPERTY_DEFINITION('material property','density of part',#7944);
#4404=PROPERTY_DEFINITION('material property','material name',#7945);
#4405=PROPERTY_DEFINITION('material property','density of part',#7945);
#4406=PROPERTY_DEFINITION('material property','material name',#7946);
#4407=PROPERTY_DEFINITION('material property','density of part',#7946);
#4408=PROPERTY_DEFINITION('material property','material name',#7947);
#4409=PROPERTY_DEFINITION('material property','density of part',#7947);
#4410=PROPERTY_DEFINITION('material property','material name',#7948);
#4411=PROPERTY_DEFINITION('material property','density of part',#7948);
#4412=PROPERTY_DEFINITION('material property','material name',#7949);
#4413=PROPERTY_DEFINITION('material property','density of part',#7949);
#4414=PROPERTY_DEFINITION('material property','material name',#7950);
#4415=PROPERTY_DEFINITION('material property','density of part',#7950);
#4416=PROPERTY_DEFINITION('material property','material name',#7951);
#4417=PROPERTY_DEFINITION('material property','density of part',#7951);
#4418=PROPERTY_DEFINITION('material property','material name',#7953);
#4419=PROPERTY_DEFINITION('material property','density of part',#7953);
#4420=PROPERTY_DEFINITION('material property','material name',#7954);
#4421=PROPERTY_DEFINITION('material property','density of part',#7954);
#4422=PROPERTY_DEFINITION('material property','material name',#7955);
#4423=PROPERTY_DEFINITION('material property','density of part',#7955);
#4424=PROPERTY_DEFINITION('material property','material name',#7956);
#4425=PROPERTY_DEFINITION('material property','density of part',#7956);
#4426=AXIS2_PLACEMENT_3D('',#6216,#4909,#4910);
#4427=AXIS2_PLACEMENT_3D('',#6217,#4911,#4912);
#4428=AXIS2_PLACEMENT_3D('',#6218,#4913,#4914);
#4429=AXIS2_PLACEMENT_3D('',#6219,#4915,#4916);
#4430=AXIS2_PLACEMENT_3D('',#6228,#4921,#4922);
#4431=AXIS2_PLACEMENT_3D('',#6234,#4926,#4927);
#4432=AXIS2_PLACEMENT_3D('',#6240,#4931,#4932);
#4433=AXIS2_PLACEMENT_3D('',#6246,#4936,#4937);
#4434=AXIS2_PLACEMENT_3D('',#6252,#4941,#4942);
#4435=AXIS2_PLACEMENT_3D('',#6258,#4946,#4947);
#4436=AXIS2_PLACEMENT_3D('',#6264,#4951,#4952);
#4437=AXIS2_PLACEMENT_3D('',#6270,#4956,#4957);
#4438=AXIS2_PLACEMENT_3D('',#6276,#4961,#4962);
#4439=AXIS2_PLACEMENT_3D('',#6285,#4967,#4968);
#4440=AXIS2_PLACEMENT_3D('',#6291,#4972,#4973);
#4441=AXIS2_PLACEMENT_3D('',#6297,#4977,#4978);
#4442=AXIS2_PLACEMENT_3D('',#6303,#4982,#4983);
#4443=AXIS2_PLACEMENT_3D('',#6309,#4987,#4988);
#4444=AXIS2_PLACEMENT_3D('',#6315,#4992,#4993);
#4445=AXIS2_PLACEMENT_3D('',#6321,#4997,#4998);
#4446=AXIS2_PLACEMENT_3D('',#6327,#5002,#5003);
#4447=AXIS2_PLACEMENT_3D('',#6333,#5007,#5008);
#4448=AXIS2_PLACEMENT_3D('',#6342,#5013,#5014);
#4449=AXIS2_PLACEMENT_3D('',#6348,#5018,#5019);
#4450=AXIS2_PLACEMENT_3D('',#6354,#5023,#5024);
#4451=AXIS2_PLACEMENT_3D('',#6360,#5028,#5029);
#4452=AXIS2_PLACEMENT_3D('',#6366,#5033,#5034);
#4453=AXIS2_PLACEMENT_3D('',#6372,#5038,#5039);
#4454=AXIS2_PLACEMENT_3D('',#6378,#5043,#5044);
#4455=AXIS2_PLACEMENT_3D('',#6384,#5048,#5049);
#4456=AXIS2_PLACEMENT_3D('',#6390,#5053,#5054);
#4457=AXIS2_PLACEMENT_3D('',#6399,#5059,#5060);
#4458=AXIS2_PLACEMENT_3D('',#6405,#5064,#5065);
#4459=AXIS2_PLACEMENT_3D('',#6411,#5069,#5070);
#4460=AXIS2_PLACEMENT_3D('',#6417,#5074,#5075);
#4461=AXIS2_PLACEMENT_3D('',#6423,#5079,#5080);
#4462=AXIS2_PLACEMENT_3D('',#6429,#5084,#5085);
#4463=AXIS2_PLACEMENT_3D('',#6435,#5089,#5090);
#4464=AXIS2_PLACEMENT_3D('',#6441,#5094,#5095);
#4465=AXIS2_PLACEMENT_3D('',#6447,#5099,#5100);
#4466=AXIS2_PLACEMENT_3D('',#6449,#5101,#5102);
#4467=AXIS2_PLACEMENT_3D('',#6452,#5104,#5105);
#4468=AXIS2_PLACEMENT_3D('',#6453,#5106,#5107);
#4469=AXIS2_PLACEMENT_3D('',#6459,#5111,#5112);
#4470=AXIS2_PLACEMENT_3D('',#6465,#5116,#5117);
#4471=AXIS2_PLACEMENT_3D('',#6468,#5120,#5121);
#4472=AXIS2_PLACEMENT_3D('',#6474,#5125,#5126);
#4473=AXIS2_PLACEMENT_3D('',#6477,#5129,#5130);
#4474=AXIS2_PLACEMENT_3D('',#6483,#5134,#5135);
#4475=AXIS2_PLACEMENT_3D('',#6486,#5138,#5139);
#4476=AXIS2_PLACEMENT_3D('',#6489,#5142,#5143);
#4477=AXIS2_PLACEMENT_3D('',#6490,#5144,#5145);
#4478=AXIS2_PLACEMENT_3D('',#6491,#5146,#5147);
#4479=AXIS2_PLACEMENT_3D('',#6492,#5148,#5149);
#4480=AXIS2_PLACEMENT_3D('',#6493,#5150,#5151);
#4481=AXIS2_PLACEMENT_3D('',#6495,#5152,#5153);
#4482=AXIS2_PLACEMENT_3D('',#6498,#5155,#5156);
#4483=AXIS2_PLACEMENT_3D('',#6499,#5157,#5158);
#4484=AXIS2_PLACEMENT_3D('',#6500,#5159,#5160);
#4485=AXIS2_PLACEMENT_3D('',#6502,#5161,#5162);
#4486=AXIS2_PLACEMENT_3D('',#6505,#5164,#5165);
#4487=AXIS2_PLACEMENT_3D('',#6506,#5166,#5167);
#4488=AXIS2_PLACEMENT_3D('',#6507,#5168,#5169);
#4489=AXIS2_PLACEMENT_3D('',#6509,#5170,#5171);
#4490=AXIS2_PLACEMENT_3D('',#6511,#5172,#5173);
#4491=AXIS2_PLACEMENT_3D('',#6512,#5174,#5175);
#4492=AXIS2_PLACEMENT_3D('',#6514,#5176,#5177);
#4493=AXIS2_PLACEMENT_3D('',#6516,#5178,#5179);
#4494=AXIS2_PLACEMENT_3D('',#6517,#5180,#5181);
#4495=AXIS2_PLACEMENT_3D('',#6519,#5183,#5184);
#4496=AXIS2_PLACEMENT_3D('',#6522,#5186,#5187);
#4497=AXIS2_PLACEMENT_3D('',#6523,#5188,#5189);
#4498=AXIS2_PLACEMENT_3D('',#6525,#5190,#5191);
#4499=AXIS2_PLACEMENT_3D('',#6527,#5193,#5194);
#4500=AXIS2_PLACEMENT_3D('',#6528,#5195,#5196);
#4501=AXIS2_PLACEMENT_3D('',#6529,#5197,#5198);
#4502=AXIS2_PLACEMENT_3D('',#6530,#5199,#5200);
#4503=AXIS2_PLACEMENT_3D('',#6535,#5202,#5203);
#4504=AXIS2_PLACEMENT_3D('',#6538,#5205,#5206);
#4505=AXIS2_PLACEMENT_3D('',#6539,#5207,#5208);
#4506=AXIS2_PLACEMENT_3D('',#6544,#5210,#5211);
#4507=AXIS2_PLACEMENT_3D('',#6547,#5213,#5214);
#4508=AXIS2_PLACEMENT_3D('',#6548,#5215,#5216);
#4509=AXIS2_PLACEMENT_3D('',#6552,#5219,#5220);
#4510=AXIS2_PLACEMENT_3D('',#6553,#5221,#5222);
#4511=AXIS2_PLACEMENT_3D('',#6558,#5224,#5225);
#4512=AXIS2_PLACEMENT_3D('',#6561,#5227,#5228);
#4513=AXIS2_PLACEMENT_3D('',#6562,#5229,#5230);
#4514=AXIS2_PLACEMENT_3D('',#6567,#5232,#5233);
#4515=AXIS2_PLACEMENT_3D('',#6570,#5235,#5236);
#4516=AXIS2_PLACEMENT_3D('',#6571,#5237,#5238);
#4517=AXIS2_PLACEMENT_3D('',#6575,#5241,#5242);
#4518=AXIS2_PLACEMENT_3D('',#6576,#5243,#5244);
#4519=AXIS2_PLACEMENT_3D('',#6588,#5251,#5252);
#4520=AXIS2_PLACEMENT_3D('',#6589,#5253,#5254);
#4521=AXIS2_PLACEMENT_3D('',#6593,#5257,#5258);
#4522=AXIS2_PLACEMENT_3D('',#6597,#5261,#5262);
#4523=AXIS2_PLACEMENT_3D('',#6599,#5264,#5265);
#4524=AXIS2_PLACEMENT_3D('',#6601,#5266,#5267);
#4525=AXIS2_PLACEMENT_3D('',#6603,#5269,#5270);
#4526=AXIS2_PLACEMENT_3D('',#6605,#5271,#5272);
#4527=AXIS2_PLACEMENT_3D('',#6607,#5274,#5275);
#4528=AXIS2_PLACEMENT_3D('',#6610,#5277,#5278);
#4529=AXIS2_PLACEMENT_3D('',#6611,#5279,#5280);
#4530=AXIS2_PLACEMENT_3D('',#6617,#5284,#5285);
#4531=AXIS2_PLACEMENT_3D('',#6626,#5290,#5291);
#4532=AXIS2_PLACEMENT_3D('',#6632,#5295,#5296);
#4533=AXIS2_PLACEMENT_3D('',#6638,#5300,#5301);
#4534=AXIS2_PLACEMENT_3D('',#6641,#5304,#5305);
#4535=AXIS2_PLACEMENT_3D('',#6643,#5307,#5308);
#4536=AXIS2_PLACEMENT_3D('',#6645,#5310,#5311);
#4537=AXIS2_PLACEMENT_3D('',#6646,#5312,#5313);
#4538=AXIS2_PLACEMENT_3D('',#6647,#5314,#5315);
#4539=AXIS2_PLACEMENT_3D('',#6652,#5317,#5318);
#4540=AXIS2_PLACEMENT_3D('',#6655,#5320,#5321);
#4541=AXIS2_PLACEMENT_3D('',#6656,#5322,#5323);
#4542=AXIS2_PLACEMENT_3D('',#6661,#5325,#5326);
#4543=AXIS2_PLACEMENT_3D('',#6664,#5328,#5329);
#4544=AXIS2_PLACEMENT_3D('',#6665,#5330,#5331);
#4545=AXIS2_PLACEMENT_3D('',#6669,#5334,#5335);
#4546=AXIS2_PLACEMENT_3D('',#6670,#5336,#5337);
#4547=AXIS2_PLACEMENT_3D('',#6675,#5339,#5340);
#4548=AXIS2_PLACEMENT_3D('',#6678,#5342,#5343);
#4549=AXIS2_PLACEMENT_3D('',#6679,#5344,#5345);
#4550=AXIS2_PLACEMENT_3D('',#6684,#5347,#5348);
#4551=AXIS2_PLACEMENT_3D('',#6687,#5350,#5351);
#4552=AXIS2_PLACEMENT_3D('',#6688,#5352,#5353);
#4553=AXIS2_PLACEMENT_3D('',#6692,#5356,#5357);
#4554=AXIS2_PLACEMENT_3D('',#6693,#5358,#5359);
#4555=AXIS2_PLACEMENT_3D('',#6705,#5366,#5367);
#4556=AXIS2_PLACEMENT_3D('',#6706,#5368,#5369);
#4557=AXIS2_PLACEMENT_3D('',#6710,#5372,#5373);
#4558=AXIS2_PLACEMENT_3D('',#6714,#5376,#5377);
#4559=AXIS2_PLACEMENT_3D('',#6716,#5379,#5380);
#4560=AXIS2_PLACEMENT_3D('',#6718,#5381,#5382);
#4561=AXIS2_PLACEMENT_3D('',#6720,#5384,#5385);
#4562=AXIS2_PLACEMENT_3D('',#6722,#5386,#5387);
#4563=AXIS2_PLACEMENT_3D('',#6724,#5389,#5390);
#4564=AXIS2_PLACEMENT_3D('',#6727,#5392,#5393);
#4565=AXIS2_PLACEMENT_3D('',#6728,#5394,#5395);
#4566=AXIS2_PLACEMENT_3D('',#6734,#5399,#5400);
#4567=AXIS2_PLACEMENT_3D('',#6743,#5405,#5406);
#4568=AXIS2_PLACEMENT_3D('',#6749,#5410,#5411);
#4569=AXIS2_PLACEMENT_3D('',#6755,#5415,#5416);
#4570=AXIS2_PLACEMENT_3D('',#6758,#5419,#5420);
#4571=AXIS2_PLACEMENT_3D('',#6760,#5422,#5423);
#4572=AXIS2_PLACEMENT_3D('',#6762,#5425,#5426);
#4573=AXIS2_PLACEMENT_3D('',#6763,#5427,#5428);
#4574=AXIS2_PLACEMENT_3D('',#6764,#5429,#5430);
#4575=AXIS2_PLACEMENT_3D('',#6773,#5435,#5436);
#4576=AXIS2_PLACEMENT_3D('',#6779,#5440,#5441);
#4577=AXIS2_PLACEMENT_3D('',#6785,#5445,#5446);
#4578=AXIS2_PLACEMENT_3D('',#6791,#5450,#5451);
#4579=AXIS2_PLACEMENT_3D('',#6797,#5455,#5456);
#4580=AXIS2_PLACEMENT_3D('',#6800,#5459,#5460);
#4581=AXIS2_PLACEMENT_3D('',#6801,#5461,#5462);
#4582=AXIS2_PLACEMENT_3D('',#6802,#5463,#5464);
#4583=AXIS2_PLACEMENT_3D('',#6804,#5465,#5466);
#4584=AXIS2_PLACEMENT_3D('',#6805,#5467,#5468);
#4585=AXIS2_PLACEMENT_3D('',#6807,#5469,#5470);
#4586=AXIS2_PLACEMENT_3D('',#6808,#5471,#5472);
#4587=AXIS2_PLACEMENT_3D('',#6810,#5473,#5474);
#4588=AXIS2_PLACEMENT_3D('',#6812,#5476,#5477);
#4589=AXIS2_PLACEMENT_3D('',#6814,#5478,#5479);
#4590=AXIS2_PLACEMENT_3D('',#6816,#5481,#5482);
#4591=AXIS2_PLACEMENT_3D('',#6818,#5483,#5484);
#4592=AXIS2_PLACEMENT_3D('',#6820,#5486,#5487);
#4593=AXIS2_PLACEMENT_3D('',#6822,#5488,#5489);
#4594=AXIS2_PLACEMENT_3D('',#6823,#5490,#5491);
#4595=AXIS2_PLACEMENT_3D('',#6825,#5492,#5493);
#4596=AXIS2_PLACEMENT_3D('',#6827,#5495,#5496);
#4597=AXIS2_PLACEMENT_3D('',#6829,#5498,#5499);
#4598=AXIS2_PLACEMENT_3D('',#6830,#5500,#5501);
#4599=AXIS2_PLACEMENT_3D('',#6839,#5506,#5507);
#4600=AXIS2_PLACEMENT_3D('',#6845,#5511,#5512);
#4601=AXIS2_PLACEMENT_3D('',#6852,#5516,#5517);
#4602=AXIS2_PLACEMENT_3D('',#6853,#5518,#5519);
#4603=AXIS2_PLACEMENT_3D('',#6867,#5527,#5528);
#4604=AXIS2_PLACEMENT_3D('',#6871,#5531,#5532);
#4605=AXIS2_PLACEMENT_3D('',#6875,#5535,#5536);
#4606=AXIS2_PLACEMENT_3D('',#6885,#5542,#5543);
#4607=AXIS2_PLACEMENT_3D('',#6887,#5545,#5546);
#4608=AXIS2_PLACEMENT_3D('',#6891,#5548,#5549);
#4609=AXIS2_PLACEMENT_3D('',#6893,#5551,#5552);
#4610=AXIS2_PLACEMENT_3D('',#6895,#5553,#5554);
#4611=AXIS2_PLACEMENT_3D('',#6898,#5556,#5557);
#4612=AXIS2_PLACEMENT_3D('',#6900,#5558,#5559);
#4613=AXIS2_PLACEMENT_3D('',#6901,#5560,#5561);
#4614=AXIS2_PLACEMENT_3D('',#6902,#5562,#5563);
#4615=AXIS2_PLACEMENT_3D('',#6904,#5565,#5566);
#4616=AXIS2_PLACEMENT_3D('',#6906,#5568,#5569);
#4617=AXIS2_PLACEMENT_3D('',#6908,#5571,#5572);
#4618=AXIS2_PLACEMENT_3D('',#6909,#5573,#5574);
#4619=AXIS2_PLACEMENT_3D('',#6910,#5575,#5576);
#4620=AXIS2_PLACEMENT_3D('',#6911,#5577,#5578);
#4621=AXIS2_PLACEMENT_3D('',#6914,#5579,#5580);
#4622=AXIS2_PLACEMENT_3D('',#6915,#5581,#5582);
#4623=AXIS2_PLACEMENT_3D('',#6917,#5583,#5584);
#4624=AXIS2_PLACEMENT_3D('',#6919,#5585,#5586);
#4625=AXIS2_PLACEMENT_3D('',#6920,#5587,#5588);
#4626=AXIS2_PLACEMENT_3D('',#6921,#5589,#5590);
#4627=AXIS2_PLACEMENT_3D('',#6924,#5592,#5593);
#4628=AXIS2_PLACEMENT_3D('',#6925,#5594,#5595);
#4629=AXIS2_PLACEMENT_3D('',#6927,#5596,#5597);
#4630=AXIS2_PLACEMENT_3D('',#6930,#5599,#5600);
#4631=AXIS2_PLACEMENT_3D('',#6931,#5601,#5602);
#4632=AXIS2_PLACEMENT_3D('',#6934,#5604,#5605);
#4633=AXIS2_PLACEMENT_3D('',#6935,#5606,#5607);
#4634=AXIS2_PLACEMENT_3D('',#6936,#5608,#5609);
#4635=AXIS2_PLACEMENT_3D('',#6938,#5610,#5611);
#4636=AXIS2_PLACEMENT_3D('',#6940,#5613,#5614);
#4637=AXIS2_PLACEMENT_3D('',#6942,#5615,#5616);
#4638=AXIS2_PLACEMENT_3D('',#6943,#5617,#5618);
#4639=AXIS2_PLACEMENT_3D('',#6945,#5620,#5621);
#4640=AXIS2_PLACEMENT_3D('',#6946,#5622,#5623);
#4641=AXIS2_PLACEMENT_3D('',#6949,#5624,#5625);
#4642=AXIS2_PLACEMENT_3D('',#6950,#5626,#5627);
#4643=AXIS2_PLACEMENT_3D('',#6952,#5628,#5629);
#4644=AXIS2_PLACEMENT_3D('',#6954,#5630,#5631);
#4645=AXIS2_PLACEMENT_3D('',#6955,#5632,#5633);
#4646=AXIS2_PLACEMENT_3D('',#6956,#5634,#5635);
#4647=AXIS2_PLACEMENT_3D('',#6958,#5636,#5637);
#4648=AXIS2_PLACEMENT_3D('',#6960,#5639,#5640);
#4649=AXIS2_PLACEMENT_3D('',#6962,#5641,#5642);
#4650=AXIS2_PLACEMENT_3D('',#6964,#5643,#5644);
#4651=AXIS2_PLACEMENT_3D('',#6965,#5645,#5646);
#4652=AXIS2_PLACEMENT_3D('',#6967,#5647,#5648);
#4653=AXIS2_PLACEMENT_3D('',#6969,#5650,#5651);
#4654=AXIS2_PLACEMENT_3D('',#6971,#5652,#5653);
#4655=AXIS2_PLACEMENT_3D('',#6973,#5655,#5656);
#4656=AXIS2_PLACEMENT_3D('',#6975,#5657,#5658);
#4657=AXIS2_PLACEMENT_3D('',#6977,#5660,#5661);
#4658=AXIS2_PLACEMENT_3D('',#6978,#5662,#5663);
#4659=AXIS2_PLACEMENT_3D('',#6980,#5665,#5666);
#4660=AXIS2_PLACEMENT_3D('',#6981,#5667,#5668);
#4661=AXIS2_PLACEMENT_3D('',#6984,#5669,#5670);
#4662=AXIS2_PLACEMENT_3D('',#6985,#5671,#5672);
#4663=AXIS2_PLACEMENT_3D('',#6988,#5673,#5674);
#4664=AXIS2_PLACEMENT_3D('',#6989,#5675,#5676);
#4665=AXIS2_PLACEMENT_3D('',#6992,#5677,#5678);
#4666=AXIS2_PLACEMENT_3D('',#6993,#5679,#5680);
#4667=AXIS2_PLACEMENT_3D('',#6996,#5681,#5682);
#4668=AXIS2_PLACEMENT_3D('',#6997,#5683,#5684);
#4669=AXIS2_PLACEMENT_3D('',#7000,#5685,#5686);
#4670=AXIS2_PLACEMENT_3D('',#7001,#5687,#5688);
#4671=AXIS2_PLACEMENT_3D('',#7004,#5689,#5690);
#4672=AXIS2_PLACEMENT_3D('',#7005,#5691,#5692);
#4673=AXIS2_PLACEMENT_3D('',#7008,#5693,#5694);
#4674=AXIS2_PLACEMENT_3D('',#7009,#5695,#5696);
#4675=AXIS2_PLACEMENT_3D('',#7012,#5697,#5698);
#4676=AXIS2_PLACEMENT_3D('',#7013,#5699,#5700);
#4677=AXIS2_PLACEMENT_3D('',#7014,#5701,#5702);
#4678=AXIS2_PLACEMENT_3D('',#7040,#5703,#5704);
#4679=AXIS2_PLACEMENT_3D('',#7064,#5705,#5706);
#4680=AXIS2_PLACEMENT_3D('',#7065,#5707,#5708);
#4681=AXIS2_PLACEMENT_3D('',#7067,#5709,#5710);
#4682=AXIS2_PLACEMENT_3D('',#7092,#5711,#5712);
#4683=AXIS2_PLACEMENT_3D('',#7117,#5713,#5714);
#4684=AXIS2_PLACEMENT_3D('',#7133,#5716,#5717);
#4685=AXIS2_PLACEMENT_3D('',#7148,#5718,#5719);
#4686=AXIS2_PLACEMENT_3D('',#7173,#5720,#5721);
#4687=AXIS2_PLACEMENT_3D('',#7198,#5722,#5723);
#4688=AXIS2_PLACEMENT_3D('',#7223,#5724,#5725);
#4689=AXIS2_PLACEMENT_3D('',#7247,#5726,#5727);
#4690=AXIS2_PLACEMENT_3D('',#7248,#5728,#5729);
#4691=AXIS2_PLACEMENT_3D('',#7250,#5730,#5731);
#4692=AXIS2_PLACEMENT_3D('',#7251,#5732,#5733);
#4693=AXIS2_PLACEMENT_3D('',#7252,#5734,#5735);
#4694=AXIS2_PLACEMENT_3D('',#7276,#5736,#5737);
#4695=AXIS2_PLACEMENT_3D('',#7277,#5738,#5739);
#4696=AXIS2_PLACEMENT_3D('',#7279,#5740,#5741);
#4697=AXIS2_PLACEMENT_3D('',#7280,#5742,#5743);
#4698=AXIS2_PLACEMENT_3D('',#7281,#5744,#5745);
#4699=AXIS2_PLACEMENT_3D('',#7305,#5746,#5747);
#4700=AXIS2_PLACEMENT_3D('',#7306,#5748,#5749);
#4701=AXIS2_PLACEMENT_3D('',#7308,#5750,#5751);
#4702=AXIS2_PLACEMENT_3D('',#7309,#5752,#5753);
#4703=AXIS2_PLACEMENT_3D('',#7310,#5754,#5755);
#4704=AXIS2_PLACEMENT_3D('',#7325,#5756,#5757);
#4705=AXIS2_PLACEMENT_3D('',#7338,#5758,#5759);
#4706=AXIS2_PLACEMENT_3D('',#7340,#5760,#5761);
#4707=AXIS2_PLACEMENT_3D('',#7341,#5762,#5763);
#4708=AXIS2_PLACEMENT_3D('',#7342,#5764,#5765);
#4709=AXIS2_PLACEMENT_3D('',#7366,#5766,#5767);
#4710=AXIS2_PLACEMENT_3D('',#7367,#5768,#5769);
#4711=AXIS2_PLACEMENT_3D('',#7369,#5770,#5771);
#4712=AXIS2_PLACEMENT_3D('',#7370,#5772,#5773);
#4713=AXIS2_PLACEMENT_3D('',#7371,#5774,#5775);
#4714=AXIS2_PLACEMENT_3D('',#7395,#5776,#5777);
#4715=AXIS2_PLACEMENT_3D('',#7396,#5778,#5779);
#4716=AXIS2_PLACEMENT_3D('',#7398,#5780,#5781);
#4717=AXIS2_PLACEMENT_3D('',#7399,#5782,#5783);
#4718=AXIS2_PLACEMENT_3D('',#7400,#5784,#5785);
#4719=AXIS2_PLACEMENT_3D('',#7424,#5786,#5787);
#4720=AXIS2_PLACEMENT_3D('',#7425,#5788,#5789);
#4721=AXIS2_PLACEMENT_3D('',#7427,#5790,#5791);
#4722=AXIS2_PLACEMENT_3D('',#7430,#5793,#5794);
#4723=AXIS2_PLACEMENT_3D('',#7454,#5795,#5796);
#4724=AXIS2_PLACEMENT_3D('',#7455,#5797,#5798);
#4725=AXIS2_PLACEMENT_3D('',#7456,#5799,#5800);
#4726=AXIS2_PLACEMENT_3D('',#7457,#5801,#5802);
#4727=AXIS2_PLACEMENT_3D('',#7458,#5803,#5804);
#4728=AXIS2_PLACEMENT_3D('',#7459,#5805,#5806);
#4729=AXIS2_PLACEMENT_3D('',#7460,#5807,#5808);
#4730=AXIS2_PLACEMENT_3D('',#7461,#5809,#5810);
#4731=AXIS2_PLACEMENT_3D('',#7462,#5811,#5812);
#4732=AXIS2_PLACEMENT_3D('',#7464,#5813,#5814);
#4733=AXIS2_PLACEMENT_3D('',#7466,#5815,#5816);
#4734=AXIS2_PLACEMENT_3D('',#7467,#5817,#5818);
#4735=AXIS2_PLACEMENT_3D('',#7469,#5819,#5820);
#4736=AXIS2_PLACEMENT_3D('',#7471,#5822,#5823);
#4737=AXIS2_PLACEMENT_3D('',#7473,#5824,#5825);
#4738=AXIS2_PLACEMENT_3D('',#7474,#5826,#5827);
#4739=AXIS2_PLACEMENT_3D('',#7476,#5829,#5830);
#4740=AXIS2_PLACEMENT_3D('',#7478,#5831,#5832);
#4741=AXIS2_PLACEMENT_3D('',#7480,#5833,#5834);
#4742=AXIS2_PLACEMENT_3D('',#7481,#5835,#5836);
#4743=AXIS2_PLACEMENT_3D('',#7483,#5837,#5838);
#4744=AXIS2_PLACEMENT_3D('',#7485,#5840,#5841);
#4745=AXIS2_PLACEMENT_3D('',#7487,#5842,#5843);
#4746=AXIS2_PLACEMENT_3D('',#7488,#5844,#5845);
#4747=AXIS2_PLACEMENT_3D('',#7490,#5847,#5848);
#4748=AXIS2_PLACEMENT_3D('',#7491,#5849,#5850);
#4749=AXIS2_PLACEMENT_3D('',#7492,#5851,#5852);
#4750=AXIS2_PLACEMENT_3D('',#7493,#5853,#5854);
#4751=AXIS2_PLACEMENT_3D('',#7494,#5855,#5856);
#4752=AXIS2_PLACEMENT_3D('',#7495,#5857,#5858);
#4753=AXIS2_PLACEMENT_3D('',#7496,#5859,#5860);
#4754=AXIS2_PLACEMENT_3D('',#7498,#5861,#5862);
#4755=AXIS2_PLACEMENT_3D('',#7501,#5864,#5865);
#4756=AXIS2_PLACEMENT_3D('',#7502,#5866,#5867);
#4757=AXIS2_PLACEMENT_3D('',#7504,#5868,#5869);
#4758=AXIS2_PLACEMENT_3D('',#7507,#5871,#5872);
#4759=AXIS2_PLACEMENT_3D('',#7508,#5873,#5874);
#4760=AXIS2_PLACEMENT_3D('',#7509,#5875,#5876);
#4761=AXIS2_PLACEMENT_3D('',#7510,#5877,#5878);
#4762=AXIS2_PLACEMENT_3D('',#7511,#5879,#5880);
#4763=AXIS2_PLACEMENT_3D('',#7513,#5881,#5882);
#4764=AXIS2_PLACEMENT_3D('',#7516,#5884,#5885);
#4765=AXIS2_PLACEMENT_3D('',#7517,#5886,#5887);
#4766=AXIS2_PLACEMENT_3D('',#7519,#5888,#5889);
#4767=AXIS2_PLACEMENT_3D('',#7522,#5891,#5892);
#4768=AXIS2_PLACEMENT_3D('',#7523,#5893,#5894);
#4769=AXIS2_PLACEMENT_3D('',#7524,#5895,#5896);
#4770=AXIS2_PLACEMENT_3D('',#7525,#5897,#5898);
#4771=AXIS2_PLACEMENT_3D('',#7526,#5899,#5900);
#4772=AXIS2_PLACEMENT_3D('',#7528,#5901,#5902);
#4773=AXIS2_PLACEMENT_3D('',#7531,#5904,#5905);
#4774=AXIS2_PLACEMENT_3D('',#7532,#5906,#5907);
#4775=AXIS2_PLACEMENT_3D('',#7534,#5908,#5909);
#4776=AXIS2_PLACEMENT_3D('',#7537,#5911,#5912);
#4777=AXIS2_PLACEMENT_3D('',#7538,#5913,#5914);
#4778=AXIS2_PLACEMENT_3D('',#7539,#5915,#5916);
#4779=AXIS2_PLACEMENT_3D('',#7540,#5917,#5918);
#4780=AXIS2_PLACEMENT_3D('',#7541,#5919,#5920);
#4781=AXIS2_PLACEMENT_3D('',#7542,#5921,#5922);
#4782=AXIS2_PLACEMENT_3D('',#7544,#5923,#5924);
#4783=AXIS2_PLACEMENT_3D('',#7547,#5926,#5927);
#4784=AXIS2_PLACEMENT_3D('',#7548,#5928,#5929);
#4785=AXIS2_PLACEMENT_3D('',#7550,#5930,#5931);
#4786=AXIS2_PLACEMENT_3D('',#7553,#5933,#5934);
#4787=AXIS2_PLACEMENT_3D('',#7554,#5935,#5936);
#4788=AXIS2_PLACEMENT_3D('',#7555,#5937,#5938);
#4789=AXIS2_PLACEMENT_3D('',#7556,#5939,#5940);
#4790=AXIS2_PLACEMENT_3D('',#7557,#5941,#5942);
#4791=AXIS2_PLACEMENT_3D('',#7559,#5943,#5944);
#4792=AXIS2_PLACEMENT_3D('',#7562,#5946,#5947);
#4793=AXIS2_PLACEMENT_3D('',#7563,#5948,#5949);
#4794=AXIS2_PLACEMENT_3D('',#7565,#5950,#5951);
#4795=AXIS2_PLACEMENT_3D('',#7568,#5953,#5954);
#4796=AXIS2_PLACEMENT_3D('',#7569,#5955,#5956);
#4797=AXIS2_PLACEMENT_3D('',#7571,#5957,#5958);
#4798=AXIS2_PLACEMENT_3D('',#7574,#5960,#5961);
#4799=AXIS2_PLACEMENT_3D('',#7575,#5962,#5963);
#4800=AXIS2_PLACEMENT_3D('',#7577,#5964,#5965);
#4801=AXIS2_PLACEMENT_3D('',#7580,#5967,#5968);
#4802=AXIS2_PLACEMENT_3D('',#7581,#5969,#5970);
#4803=AXIS2_PLACEMENT_3D('',#7583,#5971,#5972);
#4804=AXIS2_PLACEMENT_3D('',#7586,#5974,#5975);
#4805=AXIS2_PLACEMENT_3D('',#7587,#5976,#5977);
#4806=AXIS2_PLACEMENT_3D('',#7589,#5978,#5979);
#4807=AXIS2_PLACEMENT_3D('',#7590,#5980,#5981);
#4808=AXIS2_PLACEMENT_3D('',#7593,#5983,#5984);
#4809=AXIS2_PLACEMENT_3D('',#7594,#5985,#5986);
#4810=AXIS2_PLACEMENT_3D('',#7596,#5987,#5988);
#4811=AXIS2_PLACEMENT_3D('',#7599,#5990,#5991);
#4812=AXIS2_PLACEMENT_3D('',#7600,#5992,#5993);
#4813=AXIS2_PLACEMENT_3D('',#7601,#5994,#5995);
#4814=AXIS2_PLACEMENT_3D('',#7602,#5996,#5997);
#4815=AXIS2_PLACEMENT_3D('',#7603,#5998,#5999);
#4816=AXIS2_PLACEMENT_3D('',#7605,#6000,#6001);
#4817=AXIS2_PLACEMENT_3D('',#7608,#6003,#6004);
#4818=AXIS2_PLACEMENT_3D('',#7609,#6005,#6006);
#4819=AXIS2_PLACEMENT_3D('',#7611,#6007,#6008);
#4820=AXIS2_PLACEMENT_3D('',#7614,#6010,#6011);
#4821=AXIS2_PLACEMENT_3D('',#7615,#6012,#6013);
#4822=AXIS2_PLACEMENT_3D('',#7617,#6014,#6015);
#4823=AXIS2_PLACEMENT_3D('',#7620,#6017,#6018);
#4824=AXIS2_PLACEMENT_3D('',#7621,#6019,#6020);
#4825=AXIS2_PLACEMENT_3D('',#7623,#6021,#6022);
#4826=AXIS2_PLACEMENT_3D('',#7626,#6024,#6025);
#4827=AXIS2_PLACEMENT_3D('',#7627,#6026,#6027);
#4828=AXIS2_PLACEMENT_3D('',#7629,#6028,#6029);
#4829=AXIS2_PLACEMENT_3D('',#7632,#6031,#6032);
#4830=AXIS2_PLACEMENT_3D('',#7633,#6033,#6034);
#4831=AXIS2_PLACEMENT_3D('',#7635,#6035,#6036);
#4832=AXIS2_PLACEMENT_3D('',#7638,#6038,#6039);
#4833=AXIS2_PLACEMENT_3D('',#7639,#6040,#6041);
#4834=AXIS2_PLACEMENT_3D('',#7640,#6042,#6043);
#4835=AXIS2_PLACEMENT_3D('',#7641,#6044,#6045);
#4836=AXIS2_PLACEMENT_3D('',#7642,#6046,#6047);
#4837=AXIS2_PLACEMENT_3D('',#7644,#6048,#6049);
#4838=AXIS2_PLACEMENT_3D('',#7645,#6050,#6051);
#4839=AXIS2_PLACEMENT_3D('',#7647,#6052,#6053);
#4840=AXIS2_PLACEMENT_3D('',#7649,#6055,#6056);
#4841=AXIS2_PLACEMENT_3D('',#7651,#6057,#6058);
#4842=AXIS2_PLACEMENT_3D('',#7653,#6060,#6061);
#4843=AXIS2_PLACEMENT_3D('',#7655,#6062,#6063);
#4844=AXIS2_PLACEMENT_3D('',#7657,#6065,#6066);
#4845=AXIS2_PLACEMENT_3D('',#7659,#6067,#6068);
#4846=AXIS2_PLACEMENT_3D('',#7660,#6069,#6070);
#4847=AXIS2_PLACEMENT_3D('',#7662,#6071,#6072);
#4848=AXIS2_PLACEMENT_3D('',#7664,#6074,#6075);
#4849=AXIS2_PLACEMENT_3D('',#7666,#6076,#6077);
#4850=AXIS2_PLACEMENT_3D('',#7668,#6079,#6080);
#4851=AXIS2_PLACEMENT_3D('',#7670,#6081,#6082);
#4852=AXIS2_PLACEMENT_3D('',#7672,#6084,#6085);
#4853=AXIS2_PLACEMENT_3D('',#7673,#6086,#6087);
#4854=AXIS2_PLACEMENT_3D('',#7682,#6092,#6093);
#4855=AXIS2_PLACEMENT_3D('',#7688,#6097,#6098);
#4856=AXIS2_PLACEMENT_3D('',#7694,#6102,#6103);
#4857=AXIS2_PLACEMENT_3D('',#7700,#6107,#6108);
#4858=AXIS2_PLACEMENT_3D('',#7706,#6112,#6113);
#4859=AXIS2_PLACEMENT_3D('',#7709,#6116,#6117);
#4860=AXIS2_PLACEMENT_3D('',#7710,#6118,#6119);
#4861=AXIS2_PLACEMENT_3D('',#7711,#6120,#6121);
#4862=AXIS2_PLACEMENT_3D('',#7712,#6122,#6123);
#4863=AXIS2_PLACEMENT_3D('',#7713,#6124,#6125);
#4864=AXIS2_PLACEMENT_3D('',#7714,#6126,#6127);
#4865=AXIS2_PLACEMENT_3D('',#7715,#6128,#6129);
#4866=AXIS2_PLACEMENT_3D('',#7716,#6130,#6131);
#4867=AXIS2_PLACEMENT_3D('',#7717,#6132,#6133);
#4868=AXIS2_PLACEMENT_3D('',#7718,#6134,#6135);
#4869=AXIS2_PLACEMENT_3D('',#7719,#6136,#6137);
#4870=AXIS2_PLACEMENT_3D('',#7720,#6138,#6139);
#4871=AXIS2_PLACEMENT_3D('',#7721,#6140,#6141);
#4872=AXIS2_PLACEMENT_3D('',#7722,#6142,#6143);
#4873=AXIS2_PLACEMENT_3D('',#7723,#6144,#6145);
#4874=AXIS2_PLACEMENT_3D('',#7724,#6146,#6147);
#4875=AXIS2_PLACEMENT_3D('',#7725,#6148,#6149);
#4876=AXIS2_PLACEMENT_3D('',#7726,#6150,#6151);
#4877=AXIS2_PLACEMENT_3D('',#7727,#6152,#6153);
#4878=AXIS2_PLACEMENT_3D('',#7728,#6154,#6155);
#4879=AXIS2_PLACEMENT_3D('',#7729,#6156,#6157);
#4880=AXIS2_PLACEMENT_3D('',#7730,#6158,#6159);
#4881=AXIS2_PLACEMENT_3D('',#7731,#6160,#6161);
#4882=AXIS2_PLACEMENT_3D('',#7732,#6162,#6163);
#4883=AXIS2_PLACEMENT_3D('',#7733,#6164,#6165);
#4884=AXIS2_PLACEMENT_3D('',#7734,#6166,#6167);
#4885=AXIS2_PLACEMENT_3D('',#7735,#6168,#6169);
#4886=AXIS2_PLACEMENT_3D('',#7736,#6170,#6171);
#4887=AXIS2_PLACEMENT_3D('',#7737,#6172,#6173);
#4888=AXIS2_PLACEMENT_3D('',#7738,#6174,#6175);
#4889=AXIS2_PLACEMENT_3D('',#7739,#6176,#6177);
#4890=AXIS2_PLACEMENT_3D('',#7740,#6178,#6179);
#4891=AXIS2_PLACEMENT_3D('',#7741,#6180,#6181);
#4892=AXIS2_PLACEMENT_3D('',#7742,#6182,#6183);
#4893=AXIS2_PLACEMENT_3D('',#7743,#6184,#6185);
#4894=AXIS2_PLACEMENT_3D('',#7744,#6186,#6187);
#4895=AXIS2_PLACEMENT_3D('',#7745,#6188,#6189);
#4896=AXIS2_PLACEMENT_3D('',#7746,#6190,#6191);
#4897=AXIS2_PLACEMENT_3D('',#7747,#6192,#6193);
#4898=AXIS2_PLACEMENT_3D('',#7748,#6194,#6195);
#4899=AXIS2_PLACEMENT_3D('',#7749,#6196,#6197);
#4900=AXIS2_PLACEMENT_3D('',#7750,#6198,#6199);
#4901=AXIS2_PLACEMENT_3D('',#7751,#6200,#6201);
#4902=AXIS2_PLACEMENT_3D('',#7752,#6202,#6203);
#4903=AXIS2_PLACEMENT_3D('',#7753,#6204,#6205);
#4904=AXIS2_PLACEMENT_3D('',#7754,#6206,#6207);
#4905=AXIS2_PLACEMENT_3D('',#7755,#6208,#6209);
#4906=AXIS2_PLACEMENT_3D('',#7756,#6210,#6211);
#4907=AXIS2_PLACEMENT_3D('',#7757,#6212,#6213);
#4908=AXIS2_PLACEMENT_3D('',#7758,#6214,#6215);
#4909=DIRECTION('axis',(0.,0.,1.));
#4910=DIRECTION('refdir',(1.,0.,0.));
#4911=DIRECTION('axis',(0.,0.,1.));
#4912=DIRECTION('refdir',(1.,0.,0.));
#4913=DIRECTION('axis',(0.,0.,1.));
#4914=DIRECTION('refdir',(1.,0.,0.));
#4915=DIRECTION('center_axis',(0.,0.,-1.));
#4916=DIRECTION('ref_axis',(0.,1.,0.));
#4917=DIRECTION('',(0.,1.,0.));
#4918=DIRECTION('',(1.,0.,0.));
#4919=DIRECTION('',(0.,-1.,0.));
#4920=DIRECTION('',(1.,0.,0.));
#4921=DIRECTION('center_axis',(0.,1.,-8.88178419700125E-16));
#4922=DIRECTION('ref_axis',(0.,8.88178419700125E-16,1.));
#4923=DIRECTION('',(0.,8.88178419700125E-16,1.));
#4924=DIRECTION('',(1.,0.,0.));
#4925=DIRECTION('',(0.,-8.88178419700125E-16,-1.));
#4926=DIRECTION('center_axis',(0.,-7.40148683083439E-16,-1.));
#4927=DIRECTION('ref_axis',(0.,1.,-7.40148683083439E-16));
#4928=DIRECTION('',(0.,1.,-7.40148683083439E-16));
#4929=DIRECTION('',(1.,0.,0.));
#4930=DIRECTION('',(0.,-1.,7.40148683083439E-16));
#4931=DIRECTION('center_axis',(0.,-0.707106781186547,-0.707106781186548));
#4932=DIRECTION('ref_axis',(0.,0.707106781186548,-0.707106781186547));
#4933=DIRECTION('',(0.,0.707106781186548,-0.707106781186547));
#4934=DIRECTION('',(1.,0.,0.));
#4935=DIRECTION('',(0.,-0.707106781186548,0.707106781186547));
#4936=DIRECTION('center_axis',(0.,-1.,2.77555756156289E-16));
#4937=DIRECTION('ref_axis',(0.,-2.77555756156289E-16,-1.));
#4938=DIRECTION('',(0.,-2.77555756156289E-16,-1.));
#4939=DIRECTION('',(1.,0.,0.));
#4940=DIRECTION('',(0.,2.77555756156289E-16,1.));
#4941=DIRECTION('center_axis',(0.,-0.707106781186547,0.707106781186548));
#4942=DIRECTION('ref_axis',(0.,-0.707106781186548,-0.707106781186547));
#4943=DIRECTION('',(0.,-0.707106781186548,-0.707106781186547));
#4944=DIRECTION('',(1.,0.,0.));
#4945=DIRECTION('',(0.,0.707106781186548,0.707106781186547));
#4946=DIRECTION('center_axis',(0.,7.40148683083438E-16,1.));
#4947=DIRECTION('ref_axis',(0.,-1.,7.40148683083438E-16));
#4948=DIRECTION('',(0.,-1.,7.40148683083438E-16));
#4949=DIRECTION('',(1.,0.,0.));
#4950=DIRECTION('',(0.,1.,-7.40148683083438E-16));
#4951=DIRECTION('center_axis',(0.,1.,-4.44089209850063E-16));
#4952=DIRECTION('ref_axis',(0.,4.44089209850063E-16,1.));
#4953=DIRECTION('',(0.,4.44089209850063E-16,1.));
#4954=DIRECTION('',(1.,0.,0.));
#4955=DIRECTION('',(0.,-4.44089209850063E-16,-1.));
#4956=DIRECTION('center_axis',(0.,2.41352831440251E-16,1.));
#4957=DIRECTION('ref_axis',(0.,-1.,2.41352831440251E-16));
#4958=DIRECTION('',(0.,-1.,2.41352831440251E-16));
#4959=DIRECTION('',(-1.,0.,0.));
#4960=DIRECTION('',(0.,1.,-2.41352831440251E-16));
#4961=DIRECTION('center_axis',(0.,-1.,2.41352831440251E-16));
#4962=DIRECTION('ref_axis',(0.,-2.41352831440251E-16,-1.));
#4963=DIRECTION('',(0.,-2.41352831440251E-16,-1.));
#4964=DIRECTION('',(1.,0.,0.));
#4965=DIRECTION('',(0.,2.41352831440251E-16,1.));
#4966=DIRECTION('',(1.,0.,0.));
#4967=DIRECTION('center_axis',(0.,0.,-1.));
#4968=DIRECTION('ref_axis',(0.,1.,0.));
#4969=DIRECTION('',(0.,1.,0.));
#4970=DIRECTION('',(1.,0.,0.));
#4971=DIRECTION('',(0.,-1.,0.));
#4972=DIRECTION('center_axis',(0.,-1.,0.));
#4973=DIRECTION('ref_axis',(0.,0.,-1.));
#4974=DIRECTION('',(0.,0.,-1.));
#4975=DIRECTION('',(1.,0.,0.));
#4976=DIRECTION('',(0.,0.,1.));
#4977=DIRECTION('center_axis',(0.,-0.707106781186547,0.707106781186548));
#4978=DIRECTION('ref_axis',(0.,-0.707106781186548,-0.707106781186547));
#4979=DIRECTION('',(0.,-0.707106781186548,-0.707106781186547));
#4980=DIRECTION('',(1.,0.,0.));
#4981=DIRECTION('',(0.,0.707106781186548,0.707106781186547));
#4982=DIRECTION('center_axis',(0.,0.,1.));
#4983=DIRECTION('ref_axis',(0.,-1.,0.));
#4984=DIRECTION('',(0.,-1.,0.));
#4985=DIRECTION('',(1.,0.,0.));
#4986=DIRECTION('',(0.,1.,0.));
#4987=DIRECTION('center_axis',(0.,0.707106781186548,0.707106781186547));
#4988=DIRECTION('ref_axis',(0.,-0.707106781186547,0.707106781186548));
#4989=DIRECTION('',(0.,-0.707106781186547,0.707106781186548));
#4990=DIRECTION('',(1.,0.,0.));
#4991=DIRECTION('',(0.,0.707106781186547,-0.707106781186548));
#4992=DIRECTION('center_axis',(0.,1.,0.));
#4993=DIRECTION('ref_axis',(0.,0.,1.));
#4994=DIRECTION('',(0.,0.,1.));
#4995=DIRECTION('',(1.,0.,0.));
#4996=DIRECTION('',(0.,0.,-1.));
#4997=DIRECTION('center_axis',(0.,0.,-1.));
#4998=DIRECTION('ref_axis',(0.,1.,0.));
#4999=DIRECTION('',(0.,1.,0.));
#5000=DIRECTION('',(1.,0.,0.));
#5001=DIRECTION('',(0.,-1.,0.));
#5002=DIRECTION('center_axis',(0.,1.,-2.41352831440251E-16));
#5003=DIRECTION('ref_axis',(0.,2.41352831440251E-16,1.));
#5004=DIRECTION('',(0.,2.41352831440251E-16,1.));
#5005=DIRECTION('',(-1.,0.,0.));
#5006=DIRECTION('',(0.,-2.41352831440251E-16,-1.));
#5007=DIRECTION('center_axis',(0.,0.,1.));
#5008=DIRECTION('ref_axis',(0.,-1.,0.));
#5009=DIRECTION('',(0.,-1.,0.));
#5010=DIRECTION('',(1.,0.,0.));
#5011=DIRECTION('',(0.,1.,0.));
#5012=DIRECTION('',(1.,0.,0.));
#5013=DIRECTION('center_axis',(0.,-1.,0.));
#5014=DIRECTION('ref_axis',(0.,0.,-1.));
#5015=DIRECTION('',(0.,0.,-1.));
#5016=DIRECTION('',(1.,0.,0.));
#5017=DIRECTION('',(0.,0.,1.));
#5018=DIRECTION('center_axis',(0.,0.,1.));
#5019=DIRECTION('ref_axis',(0.,-1.,0.));
#5020=DIRECTION('',(0.,-1.,0.));
#5021=DIRECTION('',(1.,0.,0.));
#5022=DIRECTION('',(0.,1.,0.));
#5023=DIRECTION('center_axis',(0.,0.707106781186548,0.707106781186548));
#5024=DIRECTION('ref_axis',(0.,-0.707106781186548,0.707106781186548));
#5025=DIRECTION('',(0.,-0.707106781186548,0.707106781186548));
#5026=DIRECTION('',(1.,0.,0.));
#5027=DIRECTION('',(0.,0.707106781186548,-0.707106781186548));
#5028=DIRECTION('center_axis',(0.,1.,0.));
#5029=DIRECTION('ref_axis',(0.,0.,1.));
#5030=DIRECTION('',(0.,0.,1.));
#5031=DIRECTION('',(1.,0.,0.));
#5032=DIRECTION('',(0.,0.,-1.));
#5033=DIRECTION('center_axis',(0.,0.707106781186548,-0.707106781186547));
#5034=DIRECTION('ref_axis',(0.,0.707106781186547,0.707106781186548));
#5035=DIRECTION('',(0.,0.707106781186547,0.707106781186548));
#5036=DIRECTION('',(1.,0.,0.));
#5037=DIRECTION('',(0.,-0.707106781186547,-0.707106781186548));
#5038=DIRECTION('center_axis',(0.,-7.40148683083438E-16,-1.));
#5039=DIRECTION('ref_axis',(0.,1.,-7.40148683083438E-16));
#5040=DIRECTION('',(0.,1.,-7.40148683083438E-16));
#5041=DIRECTION('',(1.,0.,0.));
#5042=DIRECTION('',(0.,-1.,7.40148683083438E-16));
#5043=DIRECTION('center_axis',(0.,-1.,0.));
#5044=DIRECTION('ref_axis',(0.,0.,-1.));
#5045=DIRECTION('',(0.,0.,-1.));
#5046=DIRECTION('',(1.,0.,0.));
#5047=DIRECTION('',(0.,0.,1.));
#5048=DIRECTION('center_axis',(0.,0.,-1.));
#5049=DIRECTION('ref_axis',(0.,1.,0.));
#5050=DIRECTION('',(0.,1.,0.));
#5051=DIRECTION('',(-1.,0.,0.));
#5052=DIRECTION('',(0.,-1.,0.));
#5053=DIRECTION('center_axis',(0.,1.,0.));
#5054=DIRECTION('ref_axis',(0.,0.,1.));
#5055=DIRECTION('',(0.,0.,1.));
#5056=DIRECTION('',(1.,0.,0.));
#5057=DIRECTION('',(0.,0.,-1.));
#5058=DIRECTION('',(1.,0.,0.));
#5059=DIRECTION('center_axis',(0.,0.,1.));
#5060=DIRECTION('ref_axis',(0.,-1.,0.));
#5061=DIRECTION('',(0.,-1.,0.));
#5062=DIRECTION('',(1.,0.,0.));
#5063=DIRECTION('',(0.,1.,0.));
#5064=DIRECTION('center_axis',(0.,1.,0.));
#5065=DIRECTION('ref_axis',(0.,0.,1.));
#5066=DIRECTION('',(0.,0.,1.));
#5067=DIRECTION('',(1.,0.,0.));
#5068=DIRECTION('',(0.,0.,-1.));
#5069=DIRECTION('center_axis',(0.,0.707106781186547,-0.707106781186548));
#5070=DIRECTION('ref_axis',(0.,0.707106781186548,0.707106781186547));
#5071=DIRECTION('',(0.,0.707106781186548,0.707106781186547));
#5072=DIRECTION('',(1.,0.,0.));
#5073=DIRECTION('',(0.,-0.707106781186548,-0.707106781186547));
#5074=DIRECTION('center_axis',(0.,0.,-1.));
#5075=DIRECTION('ref_axis',(0.,1.,0.));
#5076=DIRECTION('',(0.,1.,0.));
#5077=DIRECTION('',(1.,0.,0.));
#5078=DIRECTION('',(0.,-1.,0.));
#5079=DIRECTION('center_axis',(0.,-0.707106781186547,-0.707106781186548));
#5080=DIRECTION('ref_axis',(0.,0.707106781186548,-0.707106781186547));
#5081=DIRECTION('',(0.,0.707106781186548,-0.707106781186547));
#5082=DIRECTION('',(1.,0.,0.));
#5083=DIRECTION('',(0.,-0.707106781186548,0.707106781186547));
#5084=DIRECTION('center_axis',(0.,-1.,0.));
#5085=DIRECTION('ref_axis',(0.,0.,-1.));
#5086=DIRECTION('',(0.,0.,-1.));
#5087=DIRECTION('',(1.,0.,0.));
#5088=DIRECTION('',(0.,0.,1.));
#5089=DIRECTION('center_axis',(0.,0.,1.));
#5090=DIRECTION('ref_axis',(0.,-1.,0.));
#5091=DIRECTION('',(0.,-1.,0.));
#5092=DIRECTION('',(1.,0.,0.));
#5093=DIRECTION('',(0.,1.,0.));
#5094=DIRECTION('center_axis',(0.,-1.,0.));
#5095=DIRECTION('ref_axis',(0.,0.,-1.));
#5096=DIRECTION('',(0.,0.,-1.));
#5097=DIRECTION('',(-1.,0.,0.));
#5098=DIRECTION('',(0.,0.,1.));
#5099=DIRECTION('center_axis',(1.,0.,0.));
#5100=DIRECTION('ref_axis',(0.,0.,-1.));
#5101=DIRECTION('center_axis',(1.,0.,0.));
#5102=DIRECTION('ref_axis',(0.,0.,-1.));
#5103=DIRECTION('',(1.,0.,0.));
#5104=DIRECTION('center_axis',(-1.,0.,0.));
#5105=DIRECTION('ref_axis',(0.,0.,-1.));
#5106=DIRECTION('center_axis',(0.,1.,0.));
#5107=DIRECTION('ref_axis',(0.,0.,1.));
#5108=DIRECTION('',(0.,0.,1.));
#5109=DIRECTION('',(1.,0.,0.));
#5110=DIRECTION('',(0.,0.,1.));
#5111=DIRECTION('center_axis',(0.,1.,0.));
#5112=DIRECTION('ref_axis',(0.,0.,1.));
#5113=DIRECTION('',(0.,0.,1.));
#5114=DIRECTION('',(1.,0.,0.));
#5115=DIRECTION('',(0.,0.,1.));
#5116=DIRECTION('center_axis',(0.,0.,-1.));
#5117=DIRECTION('ref_axis',(0.,1.,0.));
#5118=DIRECTION('',(0.,1.,0.));
#5119=DIRECTION('',(0.,1.,0.));
#5120=DIRECTION('center_axis',(0.,0.,-1.));
#5121=DIRECTION('ref_axis',(0.,1.,0.));
#5122=DIRECTION('',(0.,1.,0.));
#5123=DIRECTION('',(1.,0.,0.));
#5124=DIRECTION('',(0.,1.,0.));
#5125=DIRECTION('center_axis',(0.,-1.,0.));
#5126=DIRECTION('ref_axis',(0.,0.,-1.));
#5127=DIRECTION('',(0.,0.,-1.));
#5128=DIRECTION('',(0.,0.,-1.));
#5129=DIRECTION('center_axis',(0.,-1.,0.));
#5130=DIRECTION('ref_axis',(0.,0.,-1.));
#5131=DIRECTION('',(0.,0.,-1.));
#5132=DIRECTION('',(1.,0.,0.));
#5133=DIRECTION('',(0.,0.,-1.));
#5134=DIRECTION('center_axis',(0.,0.,1.));
#5135=DIRECTION('ref_axis',(0.,-1.,0.));
#5136=DIRECTION('',(0.,-1.,0.));
#5137=DIRECTION('',(0.,-1.,0.));
#5138=DIRECTION('center_axis',(0.,0.,1.));
#5139=DIRECTION('ref_axis',(0.,-1.,0.));
#5140=DIRECTION('',(0.,-1.,0.));
#5141=DIRECTION('',(0.,-1.,0.));
#5142=DIRECTION('center_axis',(1.,0.,0.));
#5143=DIRECTION('ref_axis',(0.,0.,-1.));
#5144=DIRECTION('center_axis',(1.,0.,0.));
#5145=DIRECTION('ref_axis',(0.,0.,-1.));
#5146=DIRECTION('axis',(0.,0.,1.));
#5147=DIRECTION('refdir',(1.,0.,0.));
#5148=DIRECTION('axis',(0.,0.,1.));
#5149=DIRECTION('refdir',(1.,0.,0.));
#5150=DIRECTION('center_axis',(0.,1.,0.));
#5151=DIRECTION('ref_axis',(1.,0.,0.));
#5152=DIRECTION('center_axis',(0.,1.,0.));
#5153=DIRECTION('ref_axis',(1.,0.,0.));
#5154=DIRECTION('',(0.,1.,0.));
#5155=DIRECTION('center_axis',(0.,-1.,0.));
#5156=DIRECTION('ref_axis',(1.,0.,0.));
#5157=DIRECTION('center_axis',(0.,1.,0.));
#5158=DIRECTION('ref_axis',(1.,0.,0.));
#5159=DIRECTION('center_axis',(0.,1.,0.));
#5160=DIRECTION('ref_axis',(1.,0.,0.));
#5161=DIRECTION('center_axis',(0.,1.,0.));
#5162=DIRECTION('ref_axis',(1.,0.,0.));
#5163=DIRECTION('',(0.,1.,0.));
#5164=DIRECTION('center_axis',(0.,1.,0.));
#5165=DIRECTION('ref_axis',(1.,0.,0.));
#5166=DIRECTION('center_axis',(0.,1.,0.));
#5167=DIRECTION('ref_axis',(1.,0.,0.));
#5168=DIRECTION('center_axis',(0.,1.,0.));
#5169=DIRECTION('ref_axis',(1.,0.,0.));
#5170=DIRECTION('center_axis',(0.,1.,0.));
#5171=DIRECTION('ref_axis',(1.,0.,0.));
#5172=DIRECTION('center_axis',(0.,1.,0.));
#5173=DIRECTION('ref_axis',(1.,0.,0.));
#5174=DIRECTION('center_axis',(0.,1.,0.));
#5175=DIRECTION('ref_axis',(1.,0.,0.));
#5176=DIRECTION('center_axis',(0.,1.,0.));
#5177=DIRECTION('ref_axis',(1.,0.,0.));
#5178=DIRECTION('center_axis',(0.,-1.,0.));
#5179=DIRECTION('ref_axis',(1.,0.,0.));
#5180=DIRECTION('center_axis',(0.,1.,0.));
#5181=DIRECTION('ref_axis',(1.,0.,0.));
#5182=DIRECTION('',(0.,-1.,0.));
#5183=DIRECTION('center_axis',(0.,1.,0.));
#5184=DIRECTION('ref_axis',(1.,0.,0.));
#5185=DIRECTION('',(0.,-1.,0.));
#5186=DIRECTION('center_axis',(0.,1.,0.));
#5187=DIRECTION('ref_axis',(1.,0.,0.));
#5188=DIRECTION('center_axis',(0.,1.,0.));
#5189=DIRECTION('ref_axis',(1.,0.,0.));
#5190=DIRECTION('center_axis',(0.,1.,0.));
#5191=DIRECTION('ref_axis',(1.,0.,0.));
#5192=DIRECTION('',(0.,-1.,0.));
#5193=DIRECTION('center_axis',(0.,1.,0.));
#5194=DIRECTION('ref_axis',(1.,0.,0.));
#5195=DIRECTION('center_axis',(0.,1.,0.));
#5196=DIRECTION('ref_axis',(1.,0.,0.));
#5197=DIRECTION('axis',(0.,0.,1.));
#5198=DIRECTION('refdir',(1.,0.,0.));
#5199=DIRECTION('center_axis',(0.,0.,1.));
#5200=DIRECTION('ref_axis',(-1.,1.22464679914735E-16,0.));
#5201=DIRECTION('',(0.,0.,-1.));
#5202=DIRECTION('center_axis',(0.,0.,-1.));
#5203=DIRECTION('ref_axis',(1.,0.,0.));
#5204=DIRECTION('',(0.,0.,1.));
#5205=DIRECTION('center_axis',(0.,0.,1.));
#5206=DIRECTION('ref_axis',(1.,0.,0.));
#5207=DIRECTION('center_axis',(0.,0.,1.));
#5208=DIRECTION('ref_axis',(1.,0.,0.));
#5209=DIRECTION('',(0.,0.,1.));
#5210=DIRECTION('center_axis',(0.,0.,1.));
#5211=DIRECTION('ref_axis',(1.,0.,0.));
#5212=DIRECTION('',(0.,0.,-1.));
#5213=DIRECTION('center_axis',(0.,0.,-1.));
#5214=DIRECTION('ref_axis',(1.,0.,0.));
#5215=DIRECTION('center_axis',(0.,0.,1.));
#5216=DIRECTION('ref_axis',(1.,0.,0.));
#5217=DIRECTION('',(1.,0.,0.));
#5218=DIRECTION('',(-1.,0.,0.));
#5219=DIRECTION('center_axis',(0.,0.,1.));
#5220=DIRECTION('ref_axis',(1.,0.,0.));
#5221=DIRECTION('center_axis',(0.,0.,1.));
#5222=DIRECTION('ref_axis',(-1.,1.22464679914735E-16,0.));
#5223=DIRECTION('',(0.,0.,-1.));
#5224=DIRECTION('center_axis',(0.,0.,-1.));
#5225=DIRECTION('ref_axis',(1.,0.,0.));
#5226=DIRECTION('',(0.,0.,1.));
#5227=DIRECTION('center_axis',(0.,0.,1.));
#5228=DIRECTION('ref_axis',(1.,0.,0.));
#5229=DIRECTION('center_axis',(0.,0.,1.));
#5230=DIRECTION('ref_axis',(1.,0.,0.));
#5231=DIRECTION('',(0.,0.,1.));
#5232=DIRECTION('center_axis',(0.,0.,1.));
#5233=DIRECTION('ref_axis',(1.,0.,0.));
#5234=DIRECTION('',(0.,0.,-1.));
#5235=DIRECTION('center_axis',(0.,0.,-1.));
#5236=DIRECTION('ref_axis',(1.,0.,0.));
#5237=DIRECTION('center_axis',(0.,0.,1.));
#5238=DIRECTION('ref_axis',(1.,0.,0.));
#5239=DIRECTION('',(1.,0.,0.));
#5240=DIRECTION('',(-1.,0.,0.));
#5241=DIRECTION('center_axis',(0.,0.,1.));
#5242=DIRECTION('ref_axis',(1.,0.,0.));
#5243=DIRECTION('center_axis',(0.,-1.,0.));
#5244=DIRECTION('ref_axis',(1.,0.,0.));
#5245=DIRECTION('',(1.,0.,0.));
#5246=DIRECTION('',(0.,0.,1.));
#5247=DIRECTION('',(1.,0.,0.));
#5248=DIRECTION('',(0.,0.,1.));
#5249=DIRECTION('',(1.,0.,0.));
#5250=DIRECTION('',(1.,0.,0.));
#5251=DIRECTION('center_axis',(0.,1.,0.));
#5252=DIRECTION('ref_axis',(1.,0.,0.));
#5253=DIRECTION('center_axis',(0.,0.,1.));
#5254=DIRECTION('ref_axis',(1.,0.,0.));
#5255=DIRECTION('',(0.,1.,0.));
#5256=DIRECTION('',(-1.,0.,0.));
#5257=DIRECTION('center_axis',(0.,0.,1.));
#5258=DIRECTION('ref_axis',(1.,0.,0.));
#5259=DIRECTION('',(-1.,0.,0.));
#5260=DIRECTION('',(0.,-1.,0.));
#5261=DIRECTION('center_axis',(0.,0.,1.));
#5262=DIRECTION('ref_axis',(1.,0.,0.));
#5263=DIRECTION('',(-1.,0.,0.));
#5264=DIRECTION('center_axis',(0.,0.,1.));
#5265=DIRECTION('ref_axis',(1.,0.,0.));
#5266=DIRECTION('center_axis',(0.,0.,1.));
#5267=DIRECTION('ref_axis',(1.,0.,0.));
#5268=DIRECTION('',(0.,0.,1.));
#5269=DIRECTION('center_axis',(0.,0.,1.));
#5270=DIRECTION('ref_axis',(1.,0.,0.));
#5271=DIRECTION('center_axis',(0.,0.,1.));
#5272=DIRECTION('ref_axis',(1.,0.,0.));
#5273=DIRECTION('',(0.,0.,1.));
#5274=DIRECTION('center_axis',(0.,1.,0.));
#5275=DIRECTION('ref_axis',(1.,0.,0.));
#5276=DIRECTION('',(0.,1.,0.));
#5277=DIRECTION('center_axis',(0.,-1.,0.));
#5278=DIRECTION('ref_axis',(1.,0.,0.));
#5279=DIRECTION('center_axis',(0.,0.,1.));
#5280=DIRECTION('ref_axis',(1.,0.,0.));
#5281=DIRECTION('',(0.,1.,0.));
#5282=DIRECTION('',(-1.,0.,0.));
#5283=DIRECTION('',(0.,1.,0.));
#5284=DIRECTION('center_axis',(0.,0.,1.));
#5285=DIRECTION('ref_axis',(1.,0.,0.));
#5286=DIRECTION('',(-1.,0.,0.));
#5287=DIRECTION('',(0.,1.,0.));
#5288=DIRECTION('',(1.,0.,0.));
#5289=DIRECTION('',(0.,1.,0.));
#5290=DIRECTION('center_axis',(0.,1.,0.));
#5291=DIRECTION('ref_axis',(0.,0.,1.));
#5292=DIRECTION('',(0.,0.,-1.));
#5293=DIRECTION('',(-1.,0.,0.));
#5294=DIRECTION('',(0.,0.,1.));
#5295=DIRECTION('center_axis',(0.,1.,0.));
#5296=DIRECTION('ref_axis',(1.,0.,0.));
#5297=DIRECTION('',(0.,0.,-1.));
#5298=DIRECTION('',(1.,0.,0.));
#5299=DIRECTION('',(0.,0.,1.));
#5300=DIRECTION('center_axis',(0.,1.,0.));
#5301=DIRECTION('ref_axis',(-1.,0.,0.));
#5302=DIRECTION('',(0.,0.,1.));
#5303=DIRECTION('',(0.,0.,1.));
#5304=DIRECTION('center_axis',(-1.,0.,0.));
#5305=DIRECTION('ref_axis',(0.,-1.,0.));
#5306=DIRECTION('',(0.,-1.,0.));
#5307=DIRECTION('center_axis',(1.,0.,0.));
#5308=DIRECTION('ref_axis',(0.,1.,0.));
#5309=DIRECTION('',(0.,1.,0.));
#5310=DIRECTION('center_axis',(0.,0.,1.));
#5311=DIRECTION('ref_axis',(1.,0.,0.));
#5312=DIRECTION('axis',(0.,0.,1.));
#5313=DIRECTION('refdir',(1.,0.,0.));
#5314=DIRECTION('center_axis',(0.,0.,1.));
#5315=DIRECTION('ref_axis',(-1.,1.22464679914735E-16,0.));
#5316=DIRECTION('',(0.,0.,-1.));
#5317=DIRECTION('center_axis',(0.,0.,-1.));
#5318=DIRECTION('ref_axis',(1.,0.,0.));
#5319=DIRECTION('',(0.,0.,1.));
#5320=DIRECTION('center_axis',(0.,0.,1.));
#5321=DIRECTION('ref_axis',(1.,0.,0.));
#5322=DIRECTION('center_axis',(0.,0.,1.));
#5323=DIRECTION('ref_axis',(1.,0.,0.));
#5324=DIRECTION('',(0.,0.,1.));
#5325=DIRECTION('center_axis',(0.,0.,1.));
#5326=DIRECTION('ref_axis',(1.,0.,0.));
#5327=DIRECTION('',(0.,0.,-1.));
#5328=DIRECTION('center_axis',(0.,0.,-1.));
#5329=DIRECTION('ref_axis',(1.,0.,0.));
#5330=DIRECTION('center_axis',(0.,0.,1.));
#5331=DIRECTION('ref_axis',(1.,0.,0.));
#5332=DIRECTION('',(1.,0.,0.));
#5333=DIRECTION('',(-1.,0.,0.));
#5334=DIRECTION('center_axis',(0.,0.,1.));
#5335=DIRECTION('ref_axis',(1.,0.,0.));
#5336=DIRECTION('center_axis',(0.,0.,1.));
#5337=DIRECTION('ref_axis',(-1.,1.22464679914735E-16,0.));
#5338=DIRECTION('',(0.,0.,-1.));
#5339=DIRECTION('center_axis',(0.,0.,-1.));
#5340=DIRECTION('ref_axis',(1.,0.,0.));
#5341=DIRECTION('',(0.,0.,1.));
#5342=DIRECTION('center_axis',(0.,0.,1.));
#5343=DIRECTION('ref_axis',(1.,0.,0.));
#5344=DIRECTION('center_axis',(0.,0.,1.));
#5345=DIRECTION('ref_axis',(1.,0.,0.));
#5346=DIRECTION('',(0.,0.,1.));
#5347=DIRECTION('center_axis',(0.,0.,1.));
#5348=DIRECTION('ref_axis',(1.,0.,0.));
#5349=DIRECTION('',(0.,0.,-1.));
#5350=DIRECTION('center_axis',(0.,0.,-1.));
#5351=DIRECTION('ref_axis',(1.,0.,0.));
#5352=DIRECTION('center_axis',(0.,0.,1.));
#5353=DIRECTION('ref_axis',(1.,0.,0.));
#5354=DIRECTION('',(1.,0.,0.));
#5355=DIRECTION('',(-1.,0.,0.));
#5356=DIRECTION('center_axis',(0.,0.,1.));
#5357=DIRECTION('ref_axis',(1.,0.,0.));
#5358=DIRECTION('center_axis',(0.,-1.,0.));
#5359=DIRECTION('ref_axis',(1.,0.,0.));
#5360=DIRECTION('',(1.,0.,0.));
#5361=DIRECTION('',(0.,0.,1.));
#5362=DIRECTION('',(1.,0.,0.));
#5363=DIRECTION('',(0.,0.,1.));
#5364=DIRECTION('',(1.,0.,0.));
#5365=DIRECTION('',(1.,0.,0.));
#5366=DIRECTION('center_axis',(0.,1.,0.));
#5367=DIRECTION('ref_axis',(1.,0.,0.));
#5368=DIRECTION('center_axis',(0.,0.,1.));
#5369=DIRECTION('ref_axis',(1.,0.,0.));
#5370=DIRECTION('',(0.,1.,0.));
#5371=DIRECTION('',(-1.,0.,0.));
#5372=DIRECTION('center_axis',(0.,0.,1.));
#5373=DIRECTION('ref_axis',(1.,0.,0.));
#5374=DIRECTION('',(-1.,0.,0.));
#5375=DIRECTION('',(0.,-1.,0.));
#5376=DIRECTION('center_axis',(0.,0.,1.));
#5377=DIRECTION('ref_axis',(1.,0.,0.));
#5378=DIRECTION('',(-1.,0.,0.));
#5379=DIRECTION('center_axis',(0.,0.,1.));
#5380=DIRECTION('ref_axis',(1.,0.,0.));
#5381=DIRECTION('center_axis',(0.,0.,1.));
#5382=DIRECTION('ref_axis',(1.,0.,0.));
#5383=DIRECTION('',(0.,0.,1.));
#5384=DIRECTION('center_axis',(0.,0.,1.));
#5385=DIRECTION('ref_axis',(1.,0.,0.));
#5386=DIRECTION('center_axis',(0.,0.,1.));
#5387=DIRECTION('ref_axis',(1.,0.,0.));
#5388=DIRECTION('',(0.,0.,1.));
#5389=DIRECTION('center_axis',(0.,1.,0.));
#5390=DIRECTION('ref_axis',(1.,0.,0.));
#5391=DIRECTION('',(0.,1.,0.));
#5392=DIRECTION('center_axis',(0.,-1.,0.));
#5393=DIRECTION('ref_axis',(1.,0.,0.));
#5394=DIRECTION('center_axis',(0.,0.,1.));
#5395=DIRECTION('ref_axis',(1.,0.,0.));
#5396=DIRECTION('',(0.,1.,0.));
#5397=DIRECTION('',(-1.,0.,0.));
#5398=DIRECTION('',(0.,1.,0.));
#5399=DIRECTION('center_axis',(0.,0.,1.));
#5400=DIRECTION('ref_axis',(1.,0.,0.));
#5401=DIRECTION('',(-1.,0.,0.));
#5402=DIRECTION('',(0.,1.,0.));
#5403=DIRECTION('',(1.,0.,0.));
#5404=DIRECTION('',(0.,1.,0.));
#5405=DIRECTION('center_axis',(0.,1.,0.));
#5406=DIRECTION('ref_axis',(0.,0.,1.));
#5407=DIRECTION('',(0.,0.,-1.));
#5408=DIRECTION('',(-1.,0.,0.));
#5409=DIRECTION('',(0.,0.,1.));
#5410=DIRECTION('center_axis',(0.,1.,0.));
#5411=DIRECTION('ref_axis',(1.,0.,0.));
#5412=DIRECTION('',(0.,0.,-1.));
#5413=DIRECTION('',(1.,0.,0.));
#5414=DIRECTION('',(0.,0.,1.));
#5415=DIRECTION('center_axis',(0.,1.,0.));
#5416=DIRECTION('ref_axis',(-1.,0.,0.));
#5417=DIRECTION('',(0.,0.,1.));
#5418=DIRECTION('',(0.,0.,1.));
#5419=DIRECTION('center_axis',(-1.,0.,0.));
#5420=DIRECTION('ref_axis',(0.,-1.,0.));
#5421=DIRECTION('',(0.,-1.,0.));
#5422=DIRECTION('center_axis',(1.,0.,0.));
#5423=DIRECTION('ref_axis',(0.,1.,0.));
#5424=DIRECTION('',(0.,1.,0.));
#5425=DIRECTION('center_axis',(0.,0.,1.));
#5426=DIRECTION('ref_axis',(1.,0.,0.));
#5427=DIRECTION('axis',(0.,0.,1.));
#5428=DIRECTION('refdir',(1.,0.,0.));
#5429=DIRECTION('center_axis',(0.866025403784439,0.,-0.5));
#5430=DIRECTION('ref_axis',(0.5,0.,0.866025403784439));
#5431=DIRECTION('',(-0.5,0.,-0.866025403784439));
#5432=DIRECTION('',(0.,-1.,0.));
#5433=DIRECTION('',(0.5,0.,0.866025403784439));
#5434=DIRECTION('',(0.,-1.,0.));
#5435=DIRECTION('center_axis',(1.20185167898973E-16,0.,-1.));
#5436=DIRECTION('ref_axis',(1.,0.,1.20185167898973E-16));
#5437=DIRECTION('',(-1.,0.,-1.20185167898973E-16));
#5438=DIRECTION('',(0.,-1.,0.));
#5439=DIRECTION('',(1.,0.,1.20185167898973E-16));
#5440=DIRECTION('center_axis',(-0.866025403784439,0.,-0.5));
#5441=DIRECTION('ref_axis',(0.5,0.,-0.866025403784439));
#5442=DIRECTION('',(-0.5,0.,0.866025403784439));
#5443=DIRECTION('',(0.,-1.,0.));
#5444=DIRECTION('',(0.5,0.,-0.866025403784439));
#5445=DIRECTION('center_axis',(-0.866025403784439,0.,0.5));
#5446=DIRECTION('ref_axis',(-0.5,0.,-0.866025403784439));
#5447=DIRECTION('',(0.5,0.,0.866025403784439));
#5448=DIRECTION('',(0.,-1.,0.));
#5449=DIRECTION('',(-0.5,0.,-0.866025403784439));
#5450=DIRECTION('center_axis',(-2.40370335797945E-16,0.,1.));
#5451=DIRECTION('ref_axis',(-1.,0.,-2.40370335797945E-16));
#5452=DIRECTION('',(1.,0.,2.40370335797945E-16));
#5453=DIRECTION('',(0.,-1.,0.));
#5454=DIRECTION('',(-1.,0.,-2.40370335797945E-16));
#5455=DIRECTION('center_axis',(0.866025403784439,0.,0.5));
#5456=DIRECTION('ref_axis',(-0.5,0.,0.866025403784439));
#5457=DIRECTION('',(0.5,0.,-0.866025403784439));
#5458=DIRECTION('',(-0.5,0.,0.866025403784439));
#5459=DIRECTION('center_axis',(0.,1.,0.));
#5460=DIRECTION('ref_axis',(1.,0.,0.));
#5461=DIRECTION('center_axis',(0.,-1.,0.));
#5462=DIRECTION('ref_axis',(0.,0.,-1.));
#5463=DIRECTION('center_axis',(0.,1.,0.));
#5464=DIRECTION('ref_axis',(1.,0.,0.));
#5465=DIRECTION('center_axis',(0.,1.,0.));
#5466=DIRECTION('ref_axis',(1.,0.,0.));
#5467=DIRECTION('center_axis',(0.,1.,0.));
#5468=DIRECTION('ref_axis',(0.,0.,1.));
#5469=DIRECTION('center_axis',(0.,-1.,0.));
#5470=DIRECTION('ref_axis',(1.,0.,0.));
#5471=DIRECTION('center_axis',(0.,-1.,0.));
#5472=DIRECTION('ref_axis',(1.,0.,0.));
#5473=DIRECTION('center_axis',(0.,-1.,0.));
#5474=DIRECTION('ref_axis',(1.,0.,0.));
#5475=DIRECTION('',(0.707106781186548,0.707106781186547,8.65956056235493E-17));
#5476=DIRECTION('center_axis',(0.,-1.,0.));
#5477=DIRECTION('ref_axis',(1.,0.,0.));
#5478=DIRECTION('center_axis',(0.,-1.,0.));
#5479=DIRECTION('ref_axis',(1.,0.,0.));
#5480=DIRECTION('',(0.,1.,0.));
#5481=DIRECTION('center_axis',(0.,1.,0.));
#5482=DIRECTION('ref_axis',(1.,0.,0.));
#5483=DIRECTION('center_axis',(0.,-1.,0.));
#5484=DIRECTION('ref_axis',(1.,0.,0.));
#5485=DIRECTION('',(-0.707106781186547,0.707106781186548,-8.65956056235493E-17));
#5486=DIRECTION('center_axis',(0.,-1.,0.));
#5487=DIRECTION('ref_axis',(0.,0.,-1.));
#5488=DIRECTION('center_axis',(0.,-1.,0.));
#5489=DIRECTION('ref_axis',(1.,0.,0.));
#5490=DIRECTION('center_axis',(0.,1.,0.));
#5491=DIRECTION('ref_axis',(1.,0.,0.));
#5492=DIRECTION('center_axis',(0.,1.,0.));
#5493=DIRECTION('ref_axis',(1.,0.,0.));
#5494=DIRECTION('',(-0.447213595499958,0.894427190999916,-5.47678698264203E-17));
#5495=DIRECTION('center_axis',(0.,-1.,0.));
#5496=DIRECTION('ref_axis',(1.,0.,0.));
#5497=DIRECTION('',(0.,1.,0.));
#5498=DIRECTION('axis',(0.,0.,1.));
#5499=DIRECTION('refdir',(1.,0.,0.));
#5500=DIRECTION('center_axis',(0.,0.,1.));
#5501=DIRECTION('ref_axis',(1.,0.,0.));
#5502=DIRECTION('',(1.,0.,0.));
#5503=DIRECTION('',(0.,-1.,0.));
#5504=DIRECTION('',(-1.,0.,0.));
#5505=DIRECTION('',(0.,1.,0.));
#5506=DIRECTION('center_axis',(0.,1.,0.));
#5507=DIRECTION('ref_axis',(-1.,0.,0.));
#5508=DIRECTION('',(0.,0.,1.));
#5509=DIRECTION('',(-1.,0.,0.));
#5510=DIRECTION('',(0.,0.,1.));
#5511=DIRECTION('center_axis',(0.,0.,1.));
#5512=DIRECTION('ref_axis',(1.,0.,0.));
#5513=DIRECTION('',(0.,-1.,0.));
#5514=DIRECTION('',(1.,0.,0.));
#5515=DIRECTION('',(0.,1.,0.));
#5516=DIRECTION('center_axis',(0.,0.,-1.));
#5517=DIRECTION('ref_axis',(1.,0.,0.));
#5518=DIRECTION('center_axis',(-1.,0.,0.));
#5519=DIRECTION('ref_axis',(0.,-1.,0.));
#5520=DIRECTION('',(0.,0.,1.));
#5521=DIRECTION('',(0.,0.707106781186548,0.707106781186548));
#5522=DIRECTION('',(0.,-1.,0.));
#5523=DIRECTION('',(0.,0.707106781186548,-0.707106781186548));
#5524=DIRECTION('',(0.,0.,1.));
#5525=DIRECTION('',(0.,-1.,0.));
#5526=DIRECTION('',(0.,0.,1.));
#5527=DIRECTION('center_axis',(0.,-1.,0.));
#5528=DIRECTION('ref_axis',(1.,0.,0.));
#5529=DIRECTION('',(1.,0.,0.));
#5530=DIRECTION('',(0.,0.,1.));
#5531=DIRECTION('center_axis',(0.,0.,1.));
#5532=DIRECTION('ref_axis',(1.,0.,0.));
#5533=DIRECTION('',(-1.,0.,0.));
#5534=DIRECTION('',(0.,1.,0.));
#5535=DIRECTION('center_axis',(1.,0.,0.));
#5536=DIRECTION('ref_axis',(0.,1.,0.));
#5537=DIRECTION('',(0.,0.,1.));
#5538=DIRECTION('',(0.,-0.707106781186548,0.707106781186548));
#5539=DIRECTION('',(0.,1.,0.));
#5540=DIRECTION('',(0.,-0.707106781186548,-0.707106781186548));
#5541=DIRECTION('',(0.,0.,1.));
#5542=DIRECTION('center_axis',(0.,-1.,0.));
#5543=DIRECTION('ref_axis',(1.,0.,0.));
#5544=DIRECTION('',(-1.,0.,0.));
#5545=DIRECTION('center_axis',(0.,-0.707106781186548,-0.707106781186548));
#5546=DIRECTION('ref_axis',(-1.,0.,0.));
#5547=DIRECTION('',(1.,0.,0.));
#5548=DIRECTION('center_axis',(0.,0.707106781186548,0.707106781186548));
#5549=DIRECTION('ref_axis',(0.,0.707106781186547,-0.707106781186547));
#5550=DIRECTION('',(1.,0.,0.));
#5551=DIRECTION('center_axis',(0.,0.,1.));
#5552=DIRECTION('ref_axis',(1.,0.,0.));
#5553=DIRECTION('center_axis',(0.,0.,-1.));
#5554=DIRECTION('ref_axis',(1.,0.,0.));
#5555=DIRECTION('',(0.,0.,1.));
#5556=DIRECTION('center_axis',(0.,0.,-1.));
#5557=DIRECTION('ref_axis',(1.,0.,0.));
#5558=DIRECTION('center_axis',(0.,-0.707106781186548,0.707106781186548));
#5559=DIRECTION('ref_axis',(0.,0.707106781186547,0.707106781186547));
#5560=DIRECTION('center_axis',(0.,0.,-1.));
#5561=DIRECTION('ref_axis',(1.,0.,0.));
#5562=DIRECTION('center_axis',(0.,0.,1.));
#5563=DIRECTION('ref_axis',(1.,0.,0.));
#5564=DIRECTION('',(-1.,0.,0.));
#5565=DIRECTION('center_axis',(0.,0.,1.));
#5566=DIRECTION('ref_axis',(1.,0.,0.));
#5567=DIRECTION('',(-1.,0.,0.));
#5568=DIRECTION('center_axis',(0.,0.707106781186548,-0.707106781186548));
#5569=DIRECTION('ref_axis',(-1.,0.,0.));
#5570=DIRECTION('',(1.,0.,0.));
#5571=DIRECTION('center_axis',(0.,1.,0.));
#5572=DIRECTION('ref_axis',(-1.,0.,0.));
#5573=DIRECTION('axis',(0.,0.,1.));
#5574=DIRECTION('refdir',(1.,0.,0.));
#5575=DIRECTION('axis',(0.,0.,1.));
#5576=DIRECTION('refdir',(1.,0.,0.));
#5577=DIRECTION('center_axis',(0.,-1.,0.));
#5578=DIRECTION('ref_axis',(0.,0.,-1.));
#5579=DIRECTION('center_axis',(0.,-1.,0.));
#5580=DIRECTION('ref_axis',(1.,0.,0.));
#5581=DIRECTION('center_axis',(0.,-1.,0.));
#5582=DIRECTION('ref_axis',(1.,0.,0.));
#5583=DIRECTION('center_axis',(1.,0.,1.22464679914735E-16));
#5584=DIRECTION('ref_axis',(-1.22464679914735E-16,0.,1.));
#5585=DIRECTION('center_axis',(0.,1.,0.));
#5586=DIRECTION('ref_axis',(1.,0.,0.));
#5587=DIRECTION('center_axis',(0.,1.,0.));
#5588=DIRECTION('ref_axis',(1.,0.,0.));
#5589=DIRECTION('center_axis',(0.,-1.,0.));
#5590=DIRECTION('ref_axis',(1.,0.,0.));
#5591=DIRECTION('',(0.,1.,0.));
#5592=DIRECTION('center_axis',(0.,-1.,0.));
#5593=DIRECTION('ref_axis',(1.,0.,0.));
#5594=DIRECTION('center_axis',(0.,-1.,0.));
#5595=DIRECTION('ref_axis',(1.,0.,0.));
#5596=DIRECTION('center_axis',(0.,-1.,0.));
#5597=DIRECTION('ref_axis',(1.,0.,0.));
#5598=DIRECTION('',(0.,1.,0.));
#5599=DIRECTION('center_axis',(0.,-1.,0.));
#5600=DIRECTION('ref_axis',(1.,0.,0.));
#5601=DIRECTION('center_axis',(0.,1.,0.));
#5602=DIRECTION('ref_axis',(1.,0.,0.));
#5603=DIRECTION('',(-0.707106781186547,0.707106781186548,-8.65956056235493E-17));
#5604=DIRECTION('center_axis',(0.,-1.,0.));
#5605=DIRECTION('ref_axis',(1.,0.,0.));
#5606=DIRECTION('center_axis',(0.,1.,0.));
#5607=DIRECTION('ref_axis',(0.,0.,1.));
#5608=DIRECTION('center_axis',(0.,-1.,0.));
#5609=DIRECTION('ref_axis',(1.,0.,0.));
#5610=DIRECTION('center_axis',(0.,-1.,0.));
#5611=DIRECTION('ref_axis',(1.,0.,0.));
#5612=DIRECTION('',(0.,1.,0.));
#5613=DIRECTION('center_axis',(0.,-1.,0.));
#5614=DIRECTION('ref_axis',(0.,0.,-1.));
#5615=DIRECTION('center_axis',(0.,-1.,0.));
#5616=DIRECTION('ref_axis',(1.,0.,0.));
#5617=DIRECTION('center_axis',(0.,-1.,0.));
#5618=DIRECTION('ref_axis',(1.,0.,0.));
#5619=DIRECTION('',(0.707106781186547,0.707106781186548,8.65956056235493E-17));
#5620=DIRECTION('axis',(0.,0.,1.));
#5621=DIRECTION('refdir',(1.,0.,0.));
#5622=DIRECTION('center_axis',(0.,-1.,0.));
#5623=DIRECTION('ref_axis',(0.,0.,-1.));
#5624=DIRECTION('center_axis',(0.,-1.,0.));
#5625=DIRECTION('ref_axis',(1.,0.,0.));
#5626=DIRECTION('center_axis',(0.,-1.,0.));
#5627=DIRECTION('ref_axis',(1.,0.,0.));
#5628=DIRECTION('center_axis',(1.,0.,1.22464679914735E-16));
#5629=DIRECTION('ref_axis',(-1.22464679914735E-16,0.,1.));
#5630=DIRECTION('center_axis',(0.,1.,0.));
#5631=DIRECTION('ref_axis',(1.,0.,0.));
#5632=DIRECTION('center_axis',(0.,1.,0.));
#5633=DIRECTION('ref_axis',(1.,0.,0.));
#5634=DIRECTION('center_axis',(0.,-1.,0.));
#5635=DIRECTION('ref_axis',(1.,0.,0.));
#5636=DIRECTION('center_axis',(0.,-1.,0.));
#5637=DIRECTION('ref_axis',(1.,0.,0.));
#5638=DIRECTION('',(0.,1.,0.));
#5639=DIRECTION('center_axis',(0.,1.,0.));
#5640=DIRECTION('ref_axis',(0.,0.,1.));
#5641=DIRECTION('center_axis',(0.,-1.,0.));
#5642=DIRECTION('ref_axis',(1.,0.,0.));
#5643=DIRECTION('center_axis',(0.,-1.,0.));
#5644=DIRECTION('ref_axis',(1.,0.,0.));
#5645=DIRECTION('center_axis',(0.,-1.,0.));
#5646=DIRECTION('ref_axis',(1.,0.,0.));
#5647=DIRECTION('center_axis',(0.,-1.,0.));
#5648=DIRECTION('ref_axis',(1.,0.,0.));
#5649=DIRECTION('',(0.707106781186548,0.707106781186547,8.65956056235494E-17));
#5650=DIRECTION('center_axis',(0.,-1.,0.));
#5651=DIRECTION('ref_axis',(1.,0.,0.));
#5652=DIRECTION('center_axis',(0.,-1.,0.));
#5653=DIRECTION('ref_axis',(1.,0.,0.));
#5654=DIRECTION('',(0.,1.,0.));
#5655=DIRECTION('center_axis',(0.,1.,0.));
#5656=DIRECTION('ref_axis',(1.,0.,0.));
#5657=DIRECTION('center_axis',(0.,-1.,0.));
#5658=DIRECTION('ref_axis',(1.,0.,0.));
#5659=DIRECTION('',(-0.707106781186548,0.707106781186547,-8.65956056235494E-17));
#5660=DIRECTION('center_axis',(0.,-1.,0.));
#5661=DIRECTION('ref_axis',(0.,0.,-1.));
#5662=DIRECTION('center_axis',(0.,-1.,0.));
#5663=DIRECTION('ref_axis',(1.,0.,0.));
#5664=DIRECTION('',(0.,1.,0.));
#5665=DIRECTION('axis',(0.,0.,1.));
#5666=DIRECTION('refdir',(1.,0.,0.));
#5667=DIRECTION('center_axis',(0.,0.,1.));
#5668=DIRECTION('ref_axis',(1.,0.,0.));
#5669=DIRECTION('center_axis',(1.22464679914735E-16,-1.,0.));
#5670=DIRECTION('ref_axis',(-1.,-1.22464679914735E-16,0.));
#5671=DIRECTION('center_axis',(0.707106781186548,0.,0.707106781186548));
#5672=DIRECTION('ref_axis',(0.707106781186548,0.,-0.707106781186548));
#5673=DIRECTION('center_axis',(8.65956056235494E-17,-1.,-8.65956056235493E-17));
#5674=DIRECTION('ref_axis',(-0.707106781186547,-1.22464679914735E-16,0.707106781186547));
#5675=DIRECTION('center_axis',(1.,0.,0.));
#5676=DIRECTION('ref_axis',(6.12323399573676E-17,0.,-1.));
#5677=DIRECTION('center_axis',(7.49879891330929E-33,-1.,-1.22464679914735E-16));
#5678=DIRECTION('ref_axis',(-6.12323399573676E-17,-1.22464679914735E-16,
1.));
#5679=DIRECTION('center_axis',(0.707106781186548,0.,-0.707106781186548));
#5680=DIRECTION('ref_axis',(-0.707106781186548,0.,-0.707106781186548));
#5681=DIRECTION('center_axis',(-8.65956056235493E-17,-1.,-8.65956056235494E-17));
#5682=DIRECTION('ref_axis',(0.707106781186547,-1.22464679914735E-16,0.707106781186547));
#5683=DIRECTION('center_axis',(0.,0.,-1.));
#5684=DIRECTION('ref_axis',(-1.,0.,-1.22464679914735E-16));
#5685=DIRECTION('center_axis',(-1.22464679914735E-16,-1.,-1.49975978266186E-32));
#5686=DIRECTION('ref_axis',(1.,-1.22464679914735E-16,1.22464679914735E-16));
#5687=DIRECTION('center_axis',(-0.707106781186547,0.,-0.707106781186548));
#5688=DIRECTION('ref_axis',(-0.707106781186548,0.,0.707106781186547));
#5689=DIRECTION('center_axis',(-8.65956056235493E-17,-1.,8.65956056235493E-17));
#5690=DIRECTION('ref_axis',(0.707106781186548,-1.22464679914735E-16,-0.707106781186547));
#5691=DIRECTION('center_axis',(-1.,0.,0.));
#5692=DIRECTION('ref_axis',(-1.83697019872103E-16,0.,1.));
#5693=DIRECTION('center_axis',(-2.24963967399279E-32,-1.,1.22464679914735E-16));
#5694=DIRECTION('ref_axis',(1.83697019872103E-16,-1.22464679914735E-16,
-1.));
#5695=DIRECTION('center_axis',(-0.707106781186548,0.,0.707106781186548));
#5696=DIRECTION('ref_axis',(0.707106781186547,0.,0.707106781186548));
#5697=DIRECTION('center_axis',(8.65956056235493E-17,-1.,8.65956056235493E-17));
#5698=DIRECTION('ref_axis',(-0.707106781186547,-1.22464679914735E-16,-0.707106781186548));
#5699=DIRECTION('axis',(0.,0.,1.));
#5700=DIRECTION('refdir',(1.,0.,0.));
#5701=DIRECTION('center_axis',(0.,0.,1.));
#5702=DIRECTION('ref_axis',(1.,0.,0.));
#5703=DIRECTION('center_axis',(0.,-1.,0.));
#5704=DIRECTION('ref_axis',(0.,0.,-1.));
#5705=DIRECTION('center_axis',(0.,-1.,0.));
#5706=DIRECTION('ref_axis',(0.,0.,-1.));
#5707=DIRECTION('center_axis',(0.,1.,0.));
#5708=DIRECTION('ref_axis',(1.,0.,0.));
#5709=DIRECTION('center_axis',(0.,1.,0.));
#5710=DIRECTION('ref_axis',(1.,0.,0.));
#5711=DIRECTION('center_axis',(0.,1.,0.));
#5712=DIRECTION('ref_axis',(1.,0.,0.));
#5713=DIRECTION('center_axis',(0.,1.,0.));
#5714=DIRECTION('ref_axis',(1.,0.,0.));
#5715=DIRECTION('',(0.,-1.,0.));
#5716=DIRECTION('center_axis',(0.,-1.,0.));
#5717=DIRECTION('ref_axis',(1.,0.,0.));
#5718=DIRECTION('center_axis',(0.,1.,0.));
#5719=DIRECTION('ref_axis',(1.,0.,0.));
#5720=DIRECTION('center_axis',(0.,1.,0.));
#5721=DIRECTION('ref_axis',(1.,0.,0.));
#5722=DIRECTION('center_axis',(0.,1.,0.));
#5723=DIRECTION('ref_axis',(1.,0.,0.));
#5724=DIRECTION('center_axis',(0.,1.,0.));
#5725=DIRECTION('ref_axis',(1.,0.,0.));
#5726=DIRECTION('center_axis',(0.,1.,0.));
#5727=DIRECTION('ref_axis',(1.,0.,0.));
#5728=DIRECTION('center_axis',(0.,1.,0.));
#5729=DIRECTION('ref_axis',(1.,0.,0.));
#5730=DIRECTION('center_axis',(0.,-1.,0.));
#5731=DIRECTION('ref_axis',(1.,0.,0.));
#5732=DIRECTION('center_axis',(0.,-1.,0.));
#5733=DIRECTION('ref_axis',(0.,0.,-1.));
#5734=DIRECTION('center_axis',(6.12323399573677E-17,0.,1.));
#5735=DIRECTION('ref_axis',(1.,0.,0.));
#5736=DIRECTION('center_axis',(0.,-1.,0.));
#5737=DIRECTION('ref_axis',(0.,0.,-1.));
#5738=DIRECTION('center_axis',(0.,1.,0.));
#5739=DIRECTION('ref_axis',(1.,0.,0.));
#5740=DIRECTION('center_axis',(0.,-1.,0.));
#5741=DIRECTION('ref_axis',(1.,0.,0.));
#5742=DIRECTION('center_axis',(0.,-1.,0.));
#5743=DIRECTION('ref_axis',(0.,0.,-1.));
#5744=DIRECTION('center_axis',(0.,0.,1.));
#5745=DIRECTION('ref_axis',(1.,0.,0.));
#5746=DIRECTION('center_axis',(0.,-1.,0.));
#5747=DIRECTION('ref_axis',(0.,0.,-1.));
#5748=DIRECTION('center_axis',(0.,1.,0.));
#5749=DIRECTION('ref_axis',(1.,0.,0.));
#5750=DIRECTION('center_axis',(0.,-1.,0.));
#5751=DIRECTION('ref_axis',(1.,0.,0.));
#5752=DIRECTION('center_axis',(0.,-1.,0.));
#5753=DIRECTION('ref_axis',(0.,0.,-1.));
#5754=DIRECTION('center_axis',(0.,0.,1.));
#5755=DIRECTION('ref_axis',(1.,0.,0.));
#5756=DIRECTION('center_axis',(0.,-1.,0.));
#5757=DIRECTION('ref_axis',(0.,0.,-1.));
#5758=DIRECTION('center_axis',(0.,1.,0.));
#5759=DIRECTION('ref_axis',(1.,0.,0.));
#5760=DIRECTION('center_axis',(0.,-1.,0.));
#5761=DIRECTION('ref_axis',(1.,0.,0.));
#5762=DIRECTION('center_axis',(0.,-1.,0.));
#5763=DIRECTION('ref_axis',(0.,0.,-1.));
#5764=DIRECTION('center_axis',(0.,0.,1.));
#5765=DIRECTION('ref_axis',(1.,0.,0.));
#5766=DIRECTION('center_axis',(0.,-1.,0.));
#5767=DIRECTION('ref_axis',(0.,0.,-1.));
#5768=DIRECTION('center_axis',(0.,1.,0.));
#5769=DIRECTION('ref_axis',(1.,0.,0.));
#5770=DIRECTION('center_axis',(0.,-1.,0.));
#5771=DIRECTION('ref_axis',(1.,0.,0.));
#5772=DIRECTION('center_axis',(0.,-1.,0.));
#5773=DIRECTION('ref_axis',(0.,0.,-1.));
#5774=DIRECTION('center_axis',(6.12323399573676E-17,0.,1.));
#5775=DIRECTION('ref_axis',(1.,0.,0.));
#5776=DIRECTION('center_axis',(0.,-1.,0.));
#5777=DIRECTION('ref_axis',(0.,0.,-1.));
#5778=DIRECTION('center_axis',(0.,1.,0.));
#5779=DIRECTION('ref_axis',(1.,0.,0.));
#5780=DIRECTION('center_axis',(0.,-1.,0.));
#5781=DIRECTION('ref_axis',(1.,0.,0.));
#5782=DIRECTION('center_axis',(0.,-1.,0.));
#5783=DIRECTION('ref_axis',(0.,0.,-1.));
#5784=DIRECTION('center_axis',(0.,0.,1.));
#5785=DIRECTION('ref_axis',(1.,0.,0.));
#5786=DIRECTION('center_axis',(0.,-1.,0.));
#5787=DIRECTION('ref_axis',(0.,0.,-1.));
#5788=DIRECTION('center_axis',(0.,1.,0.));
#5789=DIRECTION('ref_axis',(1.,0.,0.));
#5790=DIRECTION('center_axis',(0.,1.,0.));
#5791=DIRECTION('ref_axis',(1.,0.,0.));
#5792=DIRECTION('',(0.,1.,0.));
#5793=DIRECTION('center_axis',(0.,-1.,0.));
#5794=DIRECTION('ref_axis',(1.,0.,0.));
#5795=DIRECTION('center_axis',(0.,-1.,0.));
#5796=DIRECTION('ref_axis',(1.,0.,0.));
#5797=DIRECTION('center_axis',(0.,1.,0.));
#5798=DIRECTION('ref_axis',(1.,0.,0.));
#5799=DIRECTION('center_axis',(0.,-1.,0.));
#5800=DIRECTION('ref_axis',(0.,0.,-1.));
#5801=DIRECTION('center_axis',(0.,0.,1.));
#5802=DIRECTION('ref_axis',(1.,0.,0.));
#5803=DIRECTION('center_axis',(0.,-1.,0.));
#5804=DIRECTION('ref_axis',(0.,0.,-1.));
#5805=DIRECTION('center_axis',(0.,-1.,0.));
#5806=DIRECTION('ref_axis',(-1.,0.,0.));
#5807=DIRECTION('center_axis',(0.,1.,0.));
#5808=DIRECTION('ref_axis',(1.,0.,0.));
#5809=DIRECTION('axis',(0.,0.,1.));
#5810=DIRECTION('refdir',(1.,0.,0.));
#5811=DIRECTION('center_axis',(0.,1.,0.));
#5812=DIRECTION('ref_axis',(0.,0.,1.));
#5813=DIRECTION('center_axis',(0.,-1.,0.));
#5814=DIRECTION('ref_axis',(1.,0.,0.));
#5815=DIRECTION('center_axis',(0.,-1.,0.));
#5816=DIRECTION('ref_axis',(1.,0.,0.));
#5817=DIRECTION('center_axis',(0.,-1.,0.));
#5818=DIRECTION('ref_axis',(1.,0.,0.));
#5819=DIRECTION('center_axis',(0.,-1.,0.));
#5820=DIRECTION('ref_axis',(1.,0.,0.));
#5821=DIRECTION('',(0.,1.,0.));
#5822=DIRECTION('center_axis',(0.,-1.,0.));
#5823=DIRECTION('ref_axis',(0.,0.,-1.));
#5824=DIRECTION('center_axis',(0.,-1.,0.));
#5825=DIRECTION('ref_axis',(1.,0.,0.));
#5826=DIRECTION('center_axis',(0.,-1.,0.));
#5827=DIRECTION('ref_axis',(1.,0.,0.));
#5828=DIRECTION('',(0.,1.,0.));
#5829=DIRECTION('center_axis',(0.,1.,0.));
#5830=DIRECTION('ref_axis',(0.,0.,1.));
#5831=DIRECTION('center_axis',(0.,-1.,0.));
#5832=DIRECTION('ref_axis',(1.,0.,0.));
#5833=DIRECTION('center_axis',(0.,-1.,0.));
#5834=DIRECTION('ref_axis',(1.,0.,0.));
#5835=DIRECTION('center_axis',(0.,-1.,0.));
#5836=DIRECTION('ref_axis',(1.,0.,0.));
#5837=DIRECTION('center_axis',(0.,-1.,0.));
#5838=DIRECTION('ref_axis',(1.,0.,0.));
#5839=DIRECTION('',(0.,1.,0.));
#5840=DIRECTION('center_axis',(0.,-1.,0.));
#5841=DIRECTION('ref_axis',(0.,0.,-1.));
#5842=DIRECTION('center_axis',(0.,-1.,0.));
#5843=DIRECTION('ref_axis',(1.,0.,0.));
#5844=DIRECTION('center_axis',(0.,-1.,0.));
#5845=DIRECTION('ref_axis',(1.,0.,0.));
#5846=DIRECTION('',(0.,1.,0.));
#5847=DIRECTION('',(0.,0.,1.));
#5848=DIRECTION('',(1.,0.,0.));
#5849=DIRECTION('',(0.,0.,1.));
#5850=DIRECTION('',(1.,0.,0.));
#5851=DIRECTION('',(0.,0.,1.));
#5852=DIRECTION('',(1.,0.,0.));
#5853=DIRECTION('',(0.,0.,1.));
#5854=DIRECTION('',(1.,0.,0.));
#5855=DIRECTION('',(0.,0.,1.));
#5856=DIRECTION('',(1.,0.,0.));
#5857=DIRECTION('axis',(0.,0.,1.));
#5858=DIRECTION('refdir',(1.,0.,0.));
#5859=DIRECTION('center_axis',(0.,1.,0.));
#5860=DIRECTION('ref_axis',(1.,0.,0.));
#5861=DIRECTION('center_axis',(0.,-1.,0.));
#5862=DIRECTION('ref_axis',(1.,0.,0.));
#5863=DIRECTION('',(0.,-1.,0.));
#5864=DIRECTION('center_axis',(0.,-1.,0.));
#5865=DIRECTION('ref_axis',(1.,0.,0.));
#5866=DIRECTION('center_axis',(0.,1.,0.));
#5867=DIRECTION('ref_axis',(1.,0.,0.));
#5868=DIRECTION('center_axis',(0.,1.,0.));
#5869=DIRECTION('ref_axis',(1.,0.,0.));
#5870=DIRECTION('',(0.,-1.,0.));
#5871=DIRECTION('center_axis',(0.,1.,0.));
#5872=DIRECTION('ref_axis',(1.,0.,0.));
#5873=DIRECTION('center_axis',(0.,1.,0.));
#5874=DIRECTION('ref_axis',(1.,0.,0.));
#5875=DIRECTION('center_axis',(0.,1.,0.));
#5876=DIRECTION('ref_axis',(1.,0.,0.));
#5877=DIRECTION('axis',(0.,0.,1.));
#5878=DIRECTION('refdir',(1.,0.,0.));
#5879=DIRECTION('center_axis',(0.,1.,0.));
#5880=DIRECTION('ref_axis',(1.,0.,0.));
#5881=DIRECTION('center_axis',(0.,-1.,0.));
#5882=DIRECTION('ref_axis',(1.,0.,0.));
#5883=DIRECTION('',(0.,-1.,0.));
#5884=DIRECTION('center_axis',(0.,-1.,0.));
#5885=DIRECTION('ref_axis',(1.,0.,0.));
#5886=DIRECTION('center_axis',(0.,1.,0.));
#5887=DIRECTION('ref_axis',(1.,0.,0.));
#5888=DIRECTION('center_axis',(0.,1.,0.));
#5889=DIRECTION('ref_axis',(1.,0.,0.));
#5890=DIRECTION('',(0.,-1.,0.));
#5891=DIRECTION('center_axis',(0.,1.,0.));
#5892=DIRECTION('ref_axis',(1.,0.,0.));
#5893=DIRECTION('center_axis',(0.,1.,0.));
#5894=DIRECTION('ref_axis',(1.,0.,0.));
#5895=DIRECTION('center_axis',(0.,1.,0.));
#5896=DIRECTION('ref_axis',(1.,0.,0.));
#5897=DIRECTION('axis',(0.,0.,1.));
#5898=DIRECTION('refdir',(1.,0.,0.));
#5899=DIRECTION('center_axis',(0.,1.,0.));
#5900=DIRECTION('ref_axis',(1.,0.,0.));
#5901=DIRECTION('center_axis',(0.,-1.,0.));
#5902=DIRECTION('ref_axis',(1.,0.,0.));
#5903=DIRECTION('',(0.,-1.,0.));
#5904=DIRECTION('center_axis',(0.,-1.,0.));
#5905=DIRECTION('ref_axis',(1.,0.,0.));
#5906=DIRECTION('center_axis',(0.,1.,0.));
#5907=DIRECTION('ref_axis',(1.,0.,0.));
#5908=DIRECTION('center_axis',(0.,1.,0.));
#5909=DIRECTION('ref_axis',(1.,0.,0.));
#5910=DIRECTION('',(0.,-1.,0.));
#5911=DIRECTION('center_axis',(0.,1.,0.));
#5912=DIRECTION('ref_axis',(1.,0.,0.));
#5913=DIRECTION('center_axis',(0.,1.,0.));
#5914=DIRECTION('ref_axis',(1.,0.,0.));
#5915=DIRECTION('center_axis',(0.,1.,0.));
#5916=DIRECTION('ref_axis',(1.,0.,0.));
#5917=DIRECTION('axis',(0.,0.,1.));
#5918=DIRECTION('refdir',(1.,0.,0.));
#5919=DIRECTION('axis',(0.,0.,1.));
#5920=DIRECTION('refdir',(1.,0.,0.));
#5921=DIRECTION('center_axis',(0.,1.,0.));
#5922=DIRECTION('ref_axis',(1.,0.,0.));
#5923=DIRECTION('center_axis',(0.,-1.,0.));
#5924=DIRECTION('ref_axis',(1.,0.,0.));
#5925=DIRECTION('',(0.,-1.,0.));
#5926=DIRECTION('center_axis',(0.,-1.,0.));
#5927=DIRECTION('ref_axis',(1.,0.,0.));
#5928=DIRECTION('center_axis',(0.,1.,0.));
#5929=DIRECTION('ref_axis',(1.,0.,0.));
#5930=DIRECTION('center_axis',(0.,1.,0.));
#5931=DIRECTION('ref_axis',(1.,0.,0.));
#5932=DIRECTION('',(0.,-1.,0.));
#5933=DIRECTION('center_axis',(0.,1.,0.));
#5934=DIRECTION('ref_axis',(1.,0.,0.));
#5935=DIRECTION('center_axis',(0.,1.,0.));
#5936=DIRECTION('ref_axis',(1.,0.,0.));
#5937=DIRECTION('center_axis',(0.,1.,0.));
#5938=DIRECTION('ref_axis',(1.,0.,0.));
#5939=DIRECTION('axis',(0.,0.,1.));
#5940=DIRECTION('refdir',(1.,0.,0.));
#5941=DIRECTION('center_axis',(0.,1.,0.));
#5942=DIRECTION('ref_axis',(1.,0.,0.));
#5943=DIRECTION('center_axis',(0.,1.,0.));
#5944=DIRECTION('ref_axis',(1.,0.,0.));
#5945=DIRECTION('',(0.,1.,0.));
#5946=DIRECTION('center_axis',(0.,-1.,0.));
#5947=DIRECTION('ref_axis',(1.,0.,0.));
#5948=DIRECTION('center_axis',(0.,1.,0.));
#5949=DIRECTION('ref_axis',(1.,0.,0.));
#5950=DIRECTION('center_axis',(0.,1.,0.));
#5951=DIRECTION('ref_axis',(1.,0.,0.));
#5952=DIRECTION('',(0.,1.,0.));
#5953=DIRECTION('center_axis',(0.,-1.,0.));
#5954=DIRECTION('ref_axis',(1.,0.,0.));
#5955=DIRECTION('center_axis',(0.,1.,0.));
#5956=DIRECTION('ref_axis',(1.,0.,0.));
#5957=DIRECTION('center_axis',(0.,1.,0.));
#5958=DIRECTION('ref_axis',(1.,0.,0.));
#5959=DIRECTION('',(0.,1.,0.));
#5960=DIRECTION('center_axis',(0.,-1.,0.));
#5961=DIRECTION('ref_axis',(1.,0.,0.));
#5962=DIRECTION('center_axis',(0.,1.,0.));
#5963=DIRECTION('ref_axis',(1.,0.,0.));
#5964=DIRECTION('center_axis',(0.,1.,0.));
#5965=DIRECTION('ref_axis',(1.,0.,0.));
#5966=DIRECTION('',(0.,1.,0.));
#5967=DIRECTION('center_axis',(0.,-1.,0.));
#5968=DIRECTION('ref_axis',(1.,0.,0.));
#5969=DIRECTION('center_axis',(0.,1.,0.));
#5970=DIRECTION('ref_axis',(1.,0.,0.));
#5971=DIRECTION('center_axis',(0.,-1.,0.));
#5972=DIRECTION('ref_axis',(1.,0.,0.));
#5973=DIRECTION('',(0.,-1.,0.));
#5974=DIRECTION('center_axis',(0.,-1.,0.));
#5975=DIRECTION('ref_axis',(1.,0.,0.));
#5976=DIRECTION('center_axis',(0.,1.,0.));
#5977=DIRECTION('ref_axis',(1.,0.,0.));
#5978=DIRECTION('center_axis',(0.,1.,0.));
#5979=DIRECTION('ref_axis',(1.,0.,0.));
#5980=DIRECTION('center_axis',(0.,1.,0.));
#5981=DIRECTION('ref_axis',(1.,0.,0.));
#5982=DIRECTION('',(0.,-1.,0.));
#5983=DIRECTION('center_axis',(0.,-1.,0.));
#5984=DIRECTION('ref_axis',(1.,0.,0.));
#5985=DIRECTION('center_axis',(0.,1.,0.));
#5986=DIRECTION('ref_axis',(1.,0.,0.));
#5987=DIRECTION('center_axis',(0.,1.,0.));
#5988=DIRECTION('ref_axis',(1.,0.,0.));
#5989=DIRECTION('',(0.,-1.,0.));
#5990=DIRECTION('center_axis',(0.,1.,0.));
#5991=DIRECTION('ref_axis',(1.,0.,0.));
#5992=DIRECTION('center_axis',(0.,1.,0.));
#5993=DIRECTION('ref_axis',(1.,0.,0.));
#5994=DIRECTION('center_axis',(0.,1.,0.));
#5995=DIRECTION('ref_axis',(1.,0.,0.));
#5996=DIRECTION('axis',(0.,0.,1.));
#5997=DIRECTION('refdir',(1.,0.,0.));
#5998=DIRECTION('center_axis',(0.,1.,0.));
#5999=DIRECTION('ref_axis',(1.,0.,0.));
#6000=DIRECTION('center_axis',(0.,1.,0.));
#6001=DIRECTION('ref_axis',(1.,0.,0.));
#6002=DIRECTION('',(0.,1.,0.));
#6003=DIRECTION('center_axis',(0.,-1.,0.));
#6004=DIRECTION('ref_axis',(1.,0.,0.));
#6005=DIRECTION('center_axis',(0.,1.,0.));
#6006=DIRECTION('ref_axis',(1.,0.,0.));
#6007=DIRECTION('center_axis',(0.,1.,0.));
#6008=DIRECTION('ref_axis',(1.,0.,0.));
#6009=DIRECTION('',(0.,1.,0.));
#6010=DIRECTION('center_axis',(0.,-1.,0.));
#6011=DIRECTION('ref_axis',(1.,0.,0.));
#6012=DIRECTION('center_axis',(0.,1.,0.));
#6013=DIRECTION('ref_axis',(1.,0.,0.));
#6014=DIRECTION('center_axis',(0.,1.,0.));
#6015=DIRECTION('ref_axis',(1.,0.,0.));
#6016=DIRECTION('',(0.,1.,0.));
#6017=DIRECTION('center_axis',(0.,-1.,0.));
#6018=DIRECTION('ref_axis',(1.,0.,0.));
#6019=DIRECTION('center_axis',(0.,1.,0.));
#6020=DIRECTION('ref_axis',(1.,0.,0.));
#6021=DIRECTION('center_axis',(0.,1.,0.));
#6022=DIRECTION('ref_axis',(1.,0.,0.));
#6023=DIRECTION('',(0.,1.,0.));
#6024=DIRECTION('center_axis',(0.,-1.,0.));
#6025=DIRECTION('ref_axis',(1.,0.,0.));
#6026=DIRECTION('center_axis',(0.,1.,0.));
#6027=DIRECTION('ref_axis',(1.,0.,0.));
#6028=DIRECTION('center_axis',(0.,-1.,0.));
#6029=DIRECTION('ref_axis',(1.,0.,0.));
#6030=DIRECTION('',(0.,-1.,0.));
#6031=DIRECTION('center_axis',(0.,-1.,0.));
#6032=DIRECTION('ref_axis',(1.,0.,0.));
#6033=DIRECTION('center_axis',(0.,1.,0.));
#6034=DIRECTION('ref_axis',(1.,0.,0.));
#6035=DIRECTION('center_axis',(0.,1.,0.));
#6036=DIRECTION('ref_axis',(1.,0.,0.));
#6037=DIRECTION('',(0.,-1.,0.));
#6038=DIRECTION('center_axis',(0.,1.,0.));
#6039=DIRECTION('ref_axis',(1.,0.,0.));
#6040=DIRECTION('center_axis',(0.,1.,0.));
#6041=DIRECTION('ref_axis',(1.,0.,0.));
#6042=DIRECTION('center_axis',(0.,1.,0.));
#6043=DIRECTION('ref_axis',(1.,0.,0.));
#6044=DIRECTION('axis',(0.,0.,1.));
#6045=DIRECTION('refdir',(1.,0.,0.));
#6046=DIRECTION('center_axis',(0.,1.,0.));
#6047=DIRECTION('ref_axis',(0.,0.,1.));
#6048=DIRECTION('center_axis',(0.,-1.,0.));
#6049=DIRECTION('ref_axis',(1.,0.,0.));
#6050=DIRECTION('center_axis',(0.,-1.,0.));
#6051=DIRECTION('ref_axis',(1.,0.,0.));
#6052=DIRECTION('center_axis',(0.,-1.,0.));
#6053=DIRECTION('ref_axis',(1.,0.,0.));
#6054=DIRECTION('',(0.707106781186547,0.707106781186548,8.65956056235493E-17));
#6055=DIRECTION('center_axis',(0.,-1.,0.));
#6056=DIRECTION('ref_axis',(1.,0.,0.));
#6057=DIRECTION('center_axis',(0.,-1.,0.));
#6058=DIRECTION('ref_axis',(1.,0.,0.));
#6059=DIRECTION('',(0.,1.,0.));
#6060=DIRECTION('center_axis',(0.,1.,0.));
#6061=DIRECTION('ref_axis',(1.,0.,0.));
#6062=DIRECTION('center_axis',(0.,-1.,0.));
#6063=DIRECTION('ref_axis',(1.,0.,0.));
#6064=DIRECTION('',(-0.707106781186547,0.707106781186548,-8.65956056235493E-17));
#6065=DIRECTION('center_axis',(0.,-1.,0.));
#6066=DIRECTION('ref_axis',(0.,0.,-1.));
#6067=DIRECTION('center_axis',(0.,-1.,0.));
#6068=DIRECTION('ref_axis',(1.,0.,0.));
#6069=DIRECTION('center_axis',(0.,1.,0.));
#6070=DIRECTION('ref_axis',(1.,0.,0.));
#6071=DIRECTION('center_axis',(0.,1.,0.));
#6072=DIRECTION('ref_axis',(1.,0.,0.));
#6073=DIRECTION('',(-0.447213595499958,0.894427190999916,-5.47678698264203E-17));
#6074=DIRECTION('center_axis',(0.,-1.,0.));
#6075=DIRECTION('ref_axis',(1.,0.,0.));
#6076=DIRECTION('center_axis',(0.,1.,0.));
#6077=DIRECTION('ref_axis',(1.,0.,0.));
#6078=DIRECTION('',(0.,1.,0.));
#6079=DIRECTION('center_axis',(0.,1.,0.));
#6080=DIRECTION('ref_axis',(1.,0.,0.));
#6081=DIRECTION('center_axis',(0.,-1.,0.));
#6082=DIRECTION('ref_axis',(1.,0.,0.));
#6083=DIRECTION('',(-0.707106781186547,0.707106781186548,-8.65956056235493E-17));
#6084=DIRECTION('center_axis',(0.,-1.,0.));
#6085=DIRECTION('ref_axis',(0.,0.,-1.));
#6086=DIRECTION('center_axis',(0.866025403784439,0.,-0.5));
#6087=DIRECTION('ref_axis',(0.5,0.,0.866025403784439));
#6088=DIRECTION('',(-0.5,0.,-0.866025403784439));
#6089=DIRECTION('',(0.,-1.,0.));
#6090=DIRECTION('',(0.5,0.,0.866025403784439));
#6091=DIRECTION('',(0.,-1.,0.));
#6092=DIRECTION('center_axis',(1.60246890531964E-16,0.,-1.));
#6093=DIRECTION('ref_axis',(1.,0.,1.60246890531964E-16));
#6094=DIRECTION('',(-1.,0.,-1.60246890531964E-16));
#6095=DIRECTION('',(0.,-1.,0.));
#6096=DIRECTION('',(1.,0.,1.60246890531964E-16));
#6097=DIRECTION('center_axis',(-0.866025403784439,0.,-0.5));
#6098=DIRECTION('ref_axis',(0.5,0.,-0.866025403784439));
#6099=DIRECTION('',(-0.5,0.,0.866025403784439));
#6100=DIRECTION('',(0.,-1.,0.));
#6101=DIRECTION('',(0.5,0.,-0.866025403784439));
#6102=DIRECTION('center_axis',(-0.866025403784439,0.,0.5));
#6103=DIRECTION('ref_axis',(-0.5,0.,-0.866025403784439));
#6104=DIRECTION('',(0.5,0.,0.866025403784439));
#6105=DIRECTION('',(0.,-1.,0.));
#6106=DIRECTION('',(-0.5,0.,-0.866025403784439));
#6107=DIRECTION('center_axis',(-1.60246890531964E-16,0.,1.));
#6108=DIRECTION('ref_axis',(-1.,0.,-1.60246890531964E-16));
#6109=DIRECTION('',(1.,0.,1.60246890531964E-16));
#6110=DIRECTION('',(0.,-1.,0.));
#6111=DIRECTION('',(-1.,0.,-1.60246890531964E-16));
#6112=DIRECTION('center_axis',(0.866025403784439,0.,0.5));
#6113=DIRECTION('ref_axis',(-0.5,0.,0.866025403784439));
#6114=DIRECTION('',(0.5,0.,-0.866025403784439));
#6115=DIRECTION('',(-0.5,0.,0.866025403784439));
#6116=DIRECTION('center_axis',(0.,1.,0.));
#6117=DIRECTION('ref_axis',(1.,0.,0.));
#6118=DIRECTION('center_axis',(0.,-1.,0.));
#6119=DIRECTION('ref_axis',(0.,0.,-1.));
#6120=DIRECTION('',(0.,0.,1.));
#6121=DIRECTION('',(1.,0.,0.));
#6122=DIRECTION('',(0.,0.,1.));
#6123=DIRECTION('',(1.,0.,0.));
#6124=DIRECTION('',(0.,0.,1.));
#6125=DIRECTION('',(1.,0.,0.));
#6126=DIRECTION('',(0.,0.,1.));
#6127=DIRECTION('',(1.,0.,0.));
#6128=DIRECTION('',(0.,-1.,2.22044604925031E-16));
#6129=DIRECTION('',(1.,0.,0.));
#6130=DIRECTION('',(0.,0.,1.));
#6131=DIRECTION('',(1.,0.,0.));
#6132=DIRECTION('',(0.,-1.,2.22044604925031E-16));
#6133=DIRECTION('',(1.,0.,0.));
#6134=DIRECTION('',(0.,0.,1.));
#6135=DIRECTION('',(1.,0.,0.));
#6136=DIRECTION('',(0.,0.,1.));
#6137=DIRECTION('',(1.,0.,0.));
#6138=DIRECTION('',(0.,0.,1.));
#6139=DIRECTION('',(1.,0.,0.));
#6140=DIRECTION('',(0.,-1.,2.22044604925031E-16));
#6141=DIRECTION('',(1.,0.,0.));
#6142=DIRECTION('',(0.,0.,1.));
#6143=DIRECTION('',(1.,0.,0.));
#6144=DIRECTION('',(0.,-1.,2.22044604925031E-16));
#6145=DIRECTION('',(1.,0.,0.));
#6146=DIRECTION('',(0.,0.,1.));
#6147=DIRECTION('',(1.,0.,0.));
#6148=DIRECTION('',(0.,0.,1.));
#6149=DIRECTION('',(1.,0.,0.));
#6150=DIRECTION('',(0.,0.,1.));
#6151=DIRECTION('',(1.,0.,0.));
#6152=DIRECTION('',(0.,0.,1.));
#6153=DIRECTION('',(1.,0.,0.));
#6154=DIRECTION('',(0.,0.,1.));
#6155=DIRECTION('',(1.,0.,0.));
#6156=DIRECTION('',(0.,0.,1.));
#6157=DIRECTION('',(1.,0.,0.));
#6158=DIRECTION('',(0.,0.,1.));
#6159=DIRECTION('',(-1.,1.22464679914735E-16,0.));
#6160=DIRECTION('',(0.,0.,1.));
#6161=DIRECTION('',(1.,0.,0.));
#6162=DIRECTION('',(0.,0.,1.));
#6163=DIRECTION('',(1.,0.,0.));
#6164=DIRECTION('',(0.,0.,1.));
#6165=DIRECTION('',(1.,0.,0.));
#6166=DIRECTION('',(0.,0.,1.));
#6167=DIRECTION('',(1.,0.,0.));
#6168=DIRECTION('',(0.,0.,1.));
#6169=DIRECTION('',(1.,0.,0.));
#6170=DIRECTION('',(0.,0.,1.));
#6171=DIRECTION('',(1.,0.,0.));
#6172=DIRECTION('',(0.,0.,1.));
#6173=DIRECTION('',(1.,0.,0.));
#6174=DIRECTION('',(0.,0.,1.));
#6175=DIRECTION('',(1.,0.,0.));
#6176=DIRECTION('',(0.,0.,1.));
#6177=DIRECTION('',(1.,0.,0.));
#6178=DIRECTION('',(0.,0.,1.));
#6179=DIRECTION('',(1.,0.,0.));
#6180=DIRECTION('',(0.,0.,1.));
#6181=DIRECTION('',(1.,0.,0.));
#6182=DIRECTION('',(0.,0.,1.));
#6183=DIRECTION('',(-1.,1.22464679914735E-16,0.));
#6184=DIRECTION('',(0.,0.,1.));
#6185=DIRECTION('',(1.,0.,0.));
#6186=DIRECTION('',(0.,0.,1.));
#6187=DIRECTION('',(1.,0.,0.));
#6188=DIRECTION('',(0.,0.,1.));
#6189=DIRECTION('',(-1.,1.22464679914735E-16,0.));
#6190=DIRECTION('',(0.,0.,1.));
#6191=DIRECTION('',(-1.,1.22464679914735E-16,0.));
#6192=DIRECTION('',(0.,0.,1.));
#6193=DIRECTION('',(-1.,1.22464679914735E-16,0.));
#6194=DIRECTION('',(0.,0.,1.));
#6195=DIRECTION('',(-1.,1.22464679914735E-16,0.));
#6196=DIRECTION('',(0.,0.,1.));
#6197=DIRECTION('',(1.,0.,0.));
#6198=DIRECTION('',(0.,0.,1.));
#6199=DIRECTION('',(1.,0.,0.));
#6200=DIRECTION('',(0.,0.,1.));
#6201=DIRECTION('',(1.,0.,0.));
#6202=DIRECTION('',(0.,0.,1.));
#6203=DIRECTION('',(1.,0.,0.));
#6204=DIRECTION('',(0.,0.,1.));
#6205=DIRECTION('',(1.,0.,0.));
#6206=DIRECTION('',(-0.646228631990341,0.,0.763143862712589));
#6207=DIRECTION('',(0.763143862712589,0.,0.646228631990341));
#6208=DIRECTION('',(0.0733101645298909,0.,0.997309189658153));
#6209=DIRECTION('',(0.997309189658152,0.,-0.0733101645298909));
#6210=DIRECTION('',(-0.389059691955407,-6.73327156259659E-17,0.921212546644675));
#6211=DIRECTION('',(0.921212546644675,3.77478751010618E-16,0.389059691955407));
#6212=DIRECTION('',(0.00825968820950386,5.93636819105543E-18,0.999965888193534));
#6213=DIRECTION('',(0.999965888193533,-1.66533453693773E-16,-0.00825968820950387));
#6214=DIRECTION('',(-0.100241364317063,-1.16279119879959E-16,0.994963149508489));
#6215=DIRECTION('',(0.994963149508491,-5.77423289449866E-17,0.100241364317063));
#6216=CARTESIAN_POINT('',(0.,0.,0.));
#6217=CARTESIAN_POINT('',(0.,0.,0.));
#6218=CARTESIAN_POINT('',(0.,0.,0.));
#6219=CARTESIAN_POINT('Origin',(-0.1,0.82,-0.3));
#6220=CARTESIAN_POINT('',(0.,0.82,-0.3));
#6221=CARTESIAN_POINT('',(0.,1.,-0.3));
#6222=CARTESIAN_POINT('',(0.,0.41,-0.3));
#6223=CARTESIAN_POINT('',(30.,0.82,-0.3));
#6224=CARTESIAN_POINT('',(-0.1,0.82,-0.3));
#6225=CARTESIAN_POINT('',(30.,1.,-0.3));
#6226=CARTESIAN_POINT('',(30.,0.41,-0.3));
#6227=CARTESIAN_POINT('',(-0.05,1.,-0.3));
#6228=CARTESIAN_POINT('Origin',(-0.1,0.82,-0.55));
#6229=CARTESIAN_POINT('',(0.,0.82,-0.55));
#6230=CARTESIAN_POINT('',(0.,0.82,-0.275));
#6231=CARTESIAN_POINT('',(30.,0.82,-0.55));
#6232=CARTESIAN_POINT('',(-0.1,0.82,-0.55));
#6233=CARTESIAN_POINT('',(30.,0.82,-0.275));
#6234=CARTESIAN_POINT('Origin',(-0.1,0.67,-0.55));
#6235=CARTESIAN_POINT('',(0.,0.67,-0.55));
#6236=CARTESIAN_POINT('',(0.,0.335,-0.55));
#6237=CARTESIAN_POINT('',(30.,0.67,-0.55));
#6238=CARTESIAN_POINT('',(-0.1,0.67,-0.55));
#6239=CARTESIAN_POINT('',(30.,0.335,-0.55));
#6240=CARTESIAN_POINT('Origin',(-0.1,0.42,-0.3));
#6241=CARTESIAN_POINT('',(0.,0.42,-0.3));
#6242=CARTESIAN_POINT('',(0.,0.24,-0.12));
#6243=CARTESIAN_POINT('',(30.,0.42,-0.3));
#6244=CARTESIAN_POINT('',(-0.1,0.42,-0.3));
#6245=CARTESIAN_POINT('',(30.,0.24,-0.12));
#6246=CARTESIAN_POINT('Origin',(-0.1,0.42,0.3));
#6247=CARTESIAN_POINT('',(0.,0.42,0.3));
#6248=CARTESIAN_POINT('',(0.,0.42,0.15));
#6249=CARTESIAN_POINT('',(30.,0.42,0.3));
#6250=CARTESIAN_POINT('',(-0.1,0.42,0.3));
#6251=CARTESIAN_POINT('',(30.,0.42,0.15));
#6252=CARTESIAN_POINT('Origin',(-0.1,0.67,0.55));
#6253=CARTESIAN_POINT('',(0.,0.67,0.55));
#6254=CARTESIAN_POINT('',(6.93889390390723E-18,0.365,0.245));
#6255=CARTESIAN_POINT('',(30.,0.67,0.55));
#6256=CARTESIAN_POINT('',(-0.1,0.67,0.55));
#6257=CARTESIAN_POINT('',(30.,0.365,0.245));
#6258=CARTESIAN_POINT('Origin',(-0.1,0.82,0.55));
#6259=CARTESIAN_POINT('',(0.,0.82,0.55));
#6260=CARTESIAN_POINT('',(0.,0.41,0.55));
#6261=CARTESIAN_POINT('',(30.,0.82,0.55));
#6262=CARTESIAN_POINT('',(-0.1,0.82,0.55));
#6263=CARTESIAN_POINT('',(30.,0.41,0.55));
#6264=CARTESIAN_POINT('Origin',(-0.1,0.82,0.3));
#6265=CARTESIAN_POINT('',(0.,0.82,0.3));
#6266=CARTESIAN_POINT('',(0.,0.82,0.15));
#6267=CARTESIAN_POINT('',(30.,0.82,0.3));
#6268=CARTESIAN_POINT('',(-0.1,0.82,0.3));
#6269=CARTESIAN_POINT('',(30.,0.82,0.15));
#6270=CARTESIAN_POINT('Origin',(-0.1,1.05,0.3));
#6271=CARTESIAN_POINT('',(0.,1.,0.3));
#6272=CARTESIAN_POINT('',(0.,0.525,0.3));
#6273=CARTESIAN_POINT('',(30.,1.,0.3));
#6274=CARTESIAN_POINT('',(-0.05,1.,0.3));
#6275=CARTESIAN_POINT('',(30.,0.525,0.3));
#6276=CARTESIAN_POINT('Origin',(-0.1,-0.3,-0.82));
#6277=CARTESIAN_POINT('',(0.,-0.3,-0.82));
#6278=CARTESIAN_POINT('',(0.,-0.3,-1.));
#6279=CARTESIAN_POINT('',(0.,-0.3,-0.41));
#6280=CARTESIAN_POINT('',(30.,-0.3,-0.82));
#6281=CARTESIAN_POINT('',(-0.1,-0.3,-0.82));
#6282=CARTESIAN_POINT('',(30.,-0.3,-1.));
#6283=CARTESIAN_POINT('',(30.,-0.3,-0.41));
#6284=CARTESIAN_POINT('',(-0.05,-0.3,-1.));
#6285=CARTESIAN_POINT('Origin',(-0.1,-0.55,-0.82));
#6286=CARTESIAN_POINT('',(0.,-0.55,-0.82));
#6287=CARTESIAN_POINT('',(0.,-0.275,-0.82));
#6288=CARTESIAN_POINT('',(30.,-0.55,-0.82));
#6289=CARTESIAN_POINT('',(-0.1,-0.55,-0.82));
#6290=CARTESIAN_POINT('',(30.,-0.275,-0.82));
#6291=CARTESIAN_POINT('Origin',(-0.1,-0.55,-0.67));
#6292=CARTESIAN_POINT('',(0.,-0.55,-0.67));
#6293=CARTESIAN_POINT('',(0.,-0.55,-0.335));
#6294=CARTESIAN_POINT('',(30.,-0.55,-0.67));
#6295=CARTESIAN_POINT('',(-0.1,-0.55,-0.67));
#6296=CARTESIAN_POINT('',(30.,-0.55,-0.335));
#6297=CARTESIAN_POINT('Origin',(-0.1,-0.3,-0.42));
#6298=CARTESIAN_POINT('',(0.,-0.3,-0.42));
#6299=CARTESIAN_POINT('',(0.,-0.12,-0.24));
#6300=CARTESIAN_POINT('',(30.,-0.3,-0.42));
#6301=CARTESIAN_POINT('',(-0.1,-0.3,-0.42));
#6302=CARTESIAN_POINT('',(30.,-0.12,-0.24));
#6303=CARTESIAN_POINT('Origin',(-0.1,0.3,-0.42));
#6304=CARTESIAN_POINT('',(0.,0.3,-0.42));
#6305=CARTESIAN_POINT('',(0.,0.15,-0.42));
#6306=CARTESIAN_POINT('',(30.,0.3,-0.42));
#6307=CARTESIAN_POINT('',(-0.1,0.3,-0.42));
#6308=CARTESIAN_POINT('',(30.,0.15,-0.42));
#6309=CARTESIAN_POINT('Origin',(-0.1,0.55,-0.67));
#6310=CARTESIAN_POINT('',(0.,0.55,-0.67));
#6311=CARTESIAN_POINT('',(0.,0.245,-0.365));
#6312=CARTESIAN_POINT('',(30.,0.55,-0.67));
#6313=CARTESIAN_POINT('',(-0.1,0.55,-0.67));
#6314=CARTESIAN_POINT('',(30.,0.245,-0.365));
#6315=CARTESIAN_POINT('Origin',(-0.1,0.55,-0.82));
#6316=CARTESIAN_POINT('',(0.,0.55,-0.82));
#6317=CARTESIAN_POINT('',(0.,0.55,-0.41));
#6318=CARTESIAN_POINT('',(30.,0.55,-0.82));
#6319=CARTESIAN_POINT('',(-0.1,0.55,-0.82));
#6320=CARTESIAN_POINT('',(30.,0.55,-0.41));
#6321=CARTESIAN_POINT('Origin',(-0.1,0.3,-0.82));
#6322=CARTESIAN_POINT('',(0.,0.3,-0.82));
#6323=CARTESIAN_POINT('',(0.,0.15,-0.82));
#6324=CARTESIAN_POINT('',(30.,0.3,-0.82));
#6325=CARTESIAN_POINT('',(-0.1,0.3,-0.82));
#6326=CARTESIAN_POINT('',(30.,0.15,-0.82));
#6327=CARTESIAN_POINT('Origin',(-0.1,0.3,-1.05));
#6328=CARTESIAN_POINT('',(0.,0.3,-1.));
#6329=CARTESIAN_POINT('',(0.,0.3,-0.525));
#6330=CARTESIAN_POINT('',(30.,0.3,-1.));
#6331=CARTESIAN_POINT('',(-0.05,0.3,-1.));
#6332=CARTESIAN_POINT('',(30.,0.3,-0.525));
#6333=CARTESIAN_POINT('Origin',(-0.1,-0.82,0.3));
#6334=CARTESIAN_POINT('',(0.,-0.82,0.3));
#6335=CARTESIAN_POINT('',(0.,-1.,0.3));
#6336=CARTESIAN_POINT('',(0.,-0.41,0.3));
#6337=CARTESIAN_POINT('',(30.,-0.82,0.3));
#6338=CARTESIAN_POINT('',(-0.1,-0.82,0.3));
#6339=CARTESIAN_POINT('',(30.,-1.,0.3));
#6340=CARTESIAN_POINT('',(30.,-0.41,0.3));
#6341=CARTESIAN_POINT('',(-0.05,-1.,0.3));
#6342=CARTESIAN_POINT('Origin',(-0.1,-0.82,0.55));
#6343=CARTESIAN_POINT('',(0.,-0.82,0.55));
#6344=CARTESIAN_POINT('',(0.,-0.82,0.275));
#6345=CARTESIAN_POINT('',(30.,-0.82,0.55));
#6346=CARTESIAN_POINT('',(-0.1,-0.82,0.55));
#6347=CARTESIAN_POINT('',(30.,-0.82,0.275));
#6348=CARTESIAN_POINT('Origin',(-0.1,-0.67,0.55));
#6349=CARTESIAN_POINT('',(0.,-0.67,0.55));
#6350=CARTESIAN_POINT('',(0.,-0.335,0.55));
#6351=CARTESIAN_POINT('',(30.,-0.67,0.55));
#6352=CARTESIAN_POINT('',(-0.1,-0.67,0.55));
#6353=CARTESIAN_POINT('',(30.,-0.335,0.55));
#6354=CARTESIAN_POINT('Origin',(-0.1,-0.42,0.3));
#6355=CARTESIAN_POINT('',(0.,-0.42,0.3));
#6356=CARTESIAN_POINT('',(-6.93889390390723E-18,-0.24,0.12));
#6357=CARTESIAN_POINT('',(30.,-0.42,0.3));
#6358=CARTESIAN_POINT('',(-0.1,-0.42,0.3));
#6359=CARTESIAN_POINT('',(30.,-0.24,0.12));
#6360=CARTESIAN_POINT('Origin',(-0.1,-0.42,-0.3));
#6361=CARTESIAN_POINT('',(0.,-0.42,-0.3));
#6362=CARTESIAN_POINT('',(0.,-0.42,-0.15));
#6363=CARTESIAN_POINT('',(30.,-0.42,-0.3));
#6364=CARTESIAN_POINT('',(-0.1,-0.42,-0.3));
#6365=CARTESIAN_POINT('',(30.,-0.42,-0.15));
#6366=CARTESIAN_POINT('Origin',(-0.1,-0.67,-0.55));
#6367=CARTESIAN_POINT('',(0.,-0.67,-0.55));
#6368=CARTESIAN_POINT('',(0.,-0.365,-0.245));
#6369=CARTESIAN_POINT('',(30.,-0.67,-0.55));
#6370=CARTESIAN_POINT('',(-0.1,-0.67,-0.55));
#6371=CARTESIAN_POINT('',(30.,-0.365,-0.245));
#6372=CARTESIAN_POINT('Origin',(-0.1,-0.82,-0.55));
#6373=CARTESIAN_POINT('',(0.,-0.82,-0.55));
#6374=CARTESIAN_POINT('',(0.,-0.41,-0.55));
#6375=CARTESIAN_POINT('',(30.,-0.82,-0.55));
#6376=CARTESIAN_POINT('',(-0.1,-0.82,-0.55));
#6377=CARTESIAN_POINT('',(30.,-0.41,-0.55));
#6378=CARTESIAN_POINT('Origin',(-0.1,-0.82,-0.3));
#6379=CARTESIAN_POINT('',(0.,-0.82,-0.3));
#6380=CARTESIAN_POINT('',(0.,-0.82,-0.15));
#6381=CARTESIAN_POINT('',(30.,-0.82,-0.3));
#6382=CARTESIAN_POINT('',(-0.1,-0.82,-0.3));
#6383=CARTESIAN_POINT('',(30.,-0.82,-0.15));
#6384=CARTESIAN_POINT('Origin',(-0.1,-1.05,-0.3));
#6385=CARTESIAN_POINT('',(0.,-1.,-0.3));
#6386=CARTESIAN_POINT('',(0.,-0.525,-0.3));
#6387=CARTESIAN_POINT('',(30.,-1.,-0.3));
#6388=CARTESIAN_POINT('',(-0.05,-1.,-0.3));
#6389=CARTESIAN_POINT('',(30.,-0.525,-0.3));
#6390=CARTESIAN_POINT('Origin',(-0.1,0.3,0.82));
#6391=CARTESIAN_POINT('',(0.,0.3,0.82));
#6392=CARTESIAN_POINT('',(0.,0.3,1.));
#6393=CARTESIAN_POINT('',(0.,0.3,0.41));
#6394=CARTESIAN_POINT('',(30.,0.3,0.82));
#6395=CARTESIAN_POINT('',(-0.1,0.3,0.82));
#6396=CARTESIAN_POINT('',(30.,0.3,1.));
#6397=CARTESIAN_POINT('',(30.,0.3,0.41));
#6398=CARTESIAN_POINT('',(-0.05,0.3,1.));
#6399=CARTESIAN_POINT('Origin',(-0.1,0.55,0.82));
#6400=CARTESIAN_POINT('',(0.,0.55,0.82));
#6401=CARTESIAN_POINT('',(0.,0.275,0.82));
#6402=CARTESIAN_POINT('',(30.,0.55,0.82));
#6403=CARTESIAN_POINT('',(-0.1,0.55,0.82));
#6404=CARTESIAN_POINT('',(30.,0.275,0.82));
#6405=CARTESIAN_POINT('Origin',(-0.1,0.55,0.67));
#6406=CARTESIAN_POINT('',(0.,0.55,0.67));
#6407=CARTESIAN_POINT('',(0.,0.55,0.335));
#6408=CARTESIAN_POINT('',(30.,0.55,0.67));
#6409=CARTESIAN_POINT('',(-0.1,0.55,0.67));
#6410=CARTESIAN_POINT('',(30.,0.55,0.335));
#6411=CARTESIAN_POINT('Origin',(-0.1,0.3,0.42));
#6412=CARTESIAN_POINT('',(0.,0.3,0.42));
#6413=CARTESIAN_POINT('',(6.93889390390723E-18,0.12,0.24));
#6414=CARTESIAN_POINT('',(30.,0.3,0.42));
#6415=CARTESIAN_POINT('',(-0.1,0.3,0.42));
#6416=CARTESIAN_POINT('',(30.,0.12,0.24));
#6417=CARTESIAN_POINT('Origin',(-0.1,-0.3,0.42));
#6418=CARTESIAN_POINT('',(0.,-0.3,0.42));
#6419=CARTESIAN_POINT('',(0.,-0.15,0.42));
#6420=CARTESIAN_POINT('',(30.,-0.3,0.42));
#6421=CARTESIAN_POINT('',(-0.1,-0.3,0.42));
#6422=CARTESIAN_POINT('',(30.,-0.15,0.42));
#6423=CARTESIAN_POINT('Origin',(-0.1,-0.55,0.67));
#6424=CARTESIAN_POINT('',(0.,-0.55,0.67));
#6425=CARTESIAN_POINT('',(6.93889390390723E-18,-0.245,0.365));
#6426=CARTESIAN_POINT('',(30.,-0.55,0.67));
#6427=CARTESIAN_POINT('',(-0.1,-0.55,0.67));
#6428=CARTESIAN_POINT('',(30.,-0.245,0.365));
#6429=CARTESIAN_POINT('Origin',(-0.1,-0.55,0.82));
#6430=CARTESIAN_POINT('',(0.,-0.55,0.82));
#6431=CARTESIAN_POINT('',(0.,-0.55,0.41));
#6432=CARTESIAN_POINT('',(30.,-0.55,0.82));
#6433=CARTESIAN_POINT('',(-0.1,-0.55,0.82));
#6434=CARTESIAN_POINT('',(30.,-0.55,0.41));
#6435=CARTESIAN_POINT('Origin',(-0.1,-0.3,0.82));
#6436=CARTESIAN_POINT('',(0.,-0.3,0.82));
#6437=CARTESIAN_POINT('',(0.,-0.15,0.82));
#6438=CARTESIAN_POINT('',(30.,-0.3,0.82));
#6439=CARTESIAN_POINT('',(-0.1,-0.3,0.82));
#6440=CARTESIAN_POINT('',(30.,-0.15,0.82));
#6441=CARTESIAN_POINT('Origin',(-0.1,-0.3,1.05));
#6442=CARTESIAN_POINT('',(0.,-0.3,1.));
#6443=CARTESIAN_POINT('',(0.,-0.3,0.525));
#6444=CARTESIAN_POINT('',(30.,-0.3,1.));
#6445=CARTESIAN_POINT('',(-0.05,-0.3,1.));
#6446=CARTESIAN_POINT('',(30.,-0.3,0.525));
#6447=CARTESIAN_POINT('Origin',(-0.1,0.,0.));
#6448=CARTESIAN_POINT('',(0.,-2.57175827820944E-17,0.21));
#6449=CARTESIAN_POINT('Origin',(0.,0.,0.));
#6450=CARTESIAN_POINT('',(30.,2.57175827820944E-17,0.21));
#6451=CARTESIAN_POINT('',(-0.1,-2.57175827820944E-17,0.21));
#6452=CARTESIAN_POINT('Origin',(30.,0.,0.));
#6453=CARTESIAN_POINT('Origin',(0.,1.,-1.));
#6454=CARTESIAN_POINT('',(0.,1.,1.));
#6455=CARTESIAN_POINT('',(0.,1.,-1.));
#6456=CARTESIAN_POINT('',(30.,1.,1.));
#6457=CARTESIAN_POINT('',(0.,1.,1.));
#6458=CARTESIAN_POINT('',(30.,1.,-1.));
#6459=CARTESIAN_POINT('Origin',(0.,1.,-1.));
#6460=CARTESIAN_POINT('',(30.,1.,-1.));
#6461=CARTESIAN_POINT('',(30.,1.,-1.));
#6462=CARTESIAN_POINT('',(0.,1.,-1.));
#6463=CARTESIAN_POINT('',(0.,1.,-1.));
#6464=CARTESIAN_POINT('',(0.,1.,-1.));
#6465=CARTESIAN_POINT('Origin',(0.,-1.,-1.));
#6466=CARTESIAN_POINT('',(0.,-1.,-1.));
#6467=CARTESIAN_POINT('',(30.,-1.,-1.));
#6468=CARTESIAN_POINT('Origin',(0.,-1.,-1.));
#6469=CARTESIAN_POINT('',(30.,-1.,-1.));
#6470=CARTESIAN_POINT('',(30.,-1.,-1.));
#6471=CARTESIAN_POINT('',(0.,-1.,-1.));
#6472=CARTESIAN_POINT('',(0.,-1.,-1.));
#6473=CARTESIAN_POINT('',(0.,-1.,-1.));
#6474=CARTESIAN_POINT('Origin',(0.,-1.,1.));
#6475=CARTESIAN_POINT('',(0.,-1.,1.));
#6476=CARTESIAN_POINT('',(30.,-1.,1.));
#6477=CARTESIAN_POINT('Origin',(0.,-1.,1.));
#6478=CARTESIAN_POINT('',(30.,-1.,1.));
#6479=CARTESIAN_POINT('',(30.,-1.,1.));
#6480=CARTESIAN_POINT('',(0.,-1.,1.));
#6481=CARTESIAN_POINT('',(0.,-1.,1.));
#6482=CARTESIAN_POINT('',(0.,-1.,1.));
#6483=CARTESIAN_POINT('Origin',(0.,1.,1.));
#6484=CARTESIAN_POINT('',(0.,1.,1.));
#6485=CARTESIAN_POINT('',(30.,1.,1.));
#6486=CARTESIAN_POINT('Origin',(0.,1.,1.));
#6487=CARTESIAN_POINT('',(30.,1.,1.));
#6488=CARTESIAN_POINT('',(0.,1.,1.));
#6489=CARTESIAN_POINT('Origin',(30.,0.,0.));
#6490=CARTESIAN_POINT('Origin',(0.,0.,0.));
#6491=CARTESIAN_POINT('',(0.,0.,0.));
#6492=CARTESIAN_POINT('',(0.,0.,0.));
#6493=CARTESIAN_POINT('Origin',(0.,30.8,4.5));
#6494=CARTESIAN_POINT('',(-0.165,30.8,4.5));
#6495=CARTESIAN_POINT('Origin',(0.,30.8,4.5));
#6496=CARTESIAN_POINT('',(-0.165,32.5,4.5));
#6497=CARTESIAN_POINT('',(-0.165,30.8,4.5));
#6498=CARTESIAN_POINT('Origin',(0.,32.5,4.5));
#6499=CARTESIAN_POINT('Origin',(0.,30.8,4.5));
#6500=CARTESIAN_POINT('Origin',(0.,-2.6,4.5));
#6501=CARTESIAN_POINT('',(-0.165,-2.5,4.5));
#6502=CARTESIAN_POINT('Origin',(0.,-2.5,4.5));
#6503=CARTESIAN_POINT('',(-0.165,-0.8,4.5));
#6504=CARTESIAN_POINT('',(-0.165,-2.6,4.5));
#6505=CARTESIAN_POINT('Origin',(0.,-0.8,4.5));
#6506=CARTESIAN_POINT('Origin',(0.,-0.8,4.5));
#6507=CARTESIAN_POINT('Origin',(0.,29.1,4.5));
#6508=CARTESIAN_POINT('',(-0.6,29.1,4.5));
#6509=CARTESIAN_POINT('Origin',(0.,29.1,4.5));
#6510=CARTESIAN_POINT('',(-0.5,29.1,4.5));
#6511=CARTESIAN_POINT('Origin',(0.,29.1,4.5));
#6512=CARTESIAN_POINT('Origin',(0.,0.9,4.5));
#6513=CARTESIAN_POINT('',(-0.6,0.9,4.5));
#6514=CARTESIAN_POINT('Origin',(0.,0.9,4.5));
#6515=CARTESIAN_POINT('',(-0.5,0.9,4.5));
#6516=CARTESIAN_POINT('Origin',(0.,0.9,4.5));
#6517=CARTESIAN_POINT('Origin',(0.,0.9,4.5));
#6518=CARTESIAN_POINT('',(-0.6,0.9,4.5));
#6519=CARTESIAN_POINT('Origin',(0.,-2.5,4.5));
#6520=CARTESIAN_POINT('',(-0.5,-2.5,4.5));
#6521=CARTESIAN_POINT('',(-0.5,-2.5,4.5));
#6522=CARTESIAN_POINT('Origin',(0.,-2.5,4.5));
#6523=CARTESIAN_POINT('Origin',(0.,-2.5,4.5));
#6524=CARTESIAN_POINT('',(-0.5,32.5,4.5));
#6525=CARTESIAN_POINT('Origin',(0.,32.5,4.5));
#6526=CARTESIAN_POINT('',(-0.5,-2.5,4.5));
#6527=CARTESIAN_POINT('Origin',(0.,32.5,4.5));
#6528=CARTESIAN_POINT('Origin',(0.,-2.5,4.5));
#6529=CARTESIAN_POINT('',(0.,0.,0.));
#6530=CARTESIAN_POINT('Origin',(1.6,-2.,2.9));
#6531=CARTESIAN_POINT('',(1.3,-1.6,6.5));
#6532=CARTESIAN_POINT('',(1.3,-1.6,2.9));
#6533=CARTESIAN_POINT('',(1.3,-1.6,2.9));
#6534=CARTESIAN_POINT('',(1.3,-2.4,6.5));
#6535=CARTESIAN_POINT('Origin',(1.6,-2.,6.5));
#6536=CARTESIAN_POINT('',(1.3,-2.4,2.9));
#6537=CARTESIAN_POINT('',(1.3,-2.4,2.9));
#6538=CARTESIAN_POINT('Origin',(1.6,-2.,2.9));
#6539=CARTESIAN_POINT('Origin',(1.6,-2.,2.9));
#6540=CARTESIAN_POINT('',(1.9,-1.6,2.9));
#6541=CARTESIAN_POINT('',(1.9,-1.6,6.5));
#6542=CARTESIAN_POINT('',(1.9,-1.6,2.9));
#6543=CARTESIAN_POINT('',(1.9,-2.4,2.9));
#6544=CARTESIAN_POINT('Origin',(1.6,-2.,2.9));
#6545=CARTESIAN_POINT('',(1.9,-2.4,6.5));
#6546=CARTESIAN_POINT('',(1.9,-2.4,2.9));
#6547=CARTESIAN_POINT('Origin',(1.6,-2.,6.5));
#6548=CARTESIAN_POINT('Origin',(1.6,-2.,2.9));
#6549=CARTESIAN_POINT('',(3.3,-1.6,2.9));
#6550=CARTESIAN_POINT('',(1.3,-2.4,2.9));
#6551=CARTESIAN_POINT('',(1.325,-2.,2.9));
#6552=CARTESIAN_POINT('Origin',(1.6,-2.,2.9));
#6553=CARTESIAN_POINT('Origin',(4.4,-2.,2.9));
#6554=CARTESIAN_POINT('',(4.1,-1.6,6.5));
#6555=CARTESIAN_POINT('',(4.1,-1.6,2.9));
#6556=CARTESIAN_POINT('',(4.1,-1.6,2.9));
#6557=CARTESIAN_POINT('',(4.1,-2.4,6.5));
#6558=CARTESIAN_POINT('Origin',(4.4,-2.,6.5));
#6559=CARTESIAN_POINT('',(4.1,-2.4,2.9));
#6560=CARTESIAN_POINT('',(4.1,-2.4,2.9));
#6561=CARTESIAN_POINT('Origin',(4.4,-2.,2.9));
#6562=CARTESIAN_POINT('Origin',(4.4,-2.,2.9));
#6563=CARTESIAN_POINT('',(4.7,-1.6,2.9));
#6564=CARTESIAN_POINT('',(4.7,-1.6,6.5));
#6565=CARTESIAN_POINT('',(4.7,-1.6,2.9));
#6566=CARTESIAN_POINT('',(4.7,-2.4,2.9));
#6567=CARTESIAN_POINT('Origin',(4.4,-2.,2.9));
#6568=CARTESIAN_POINT('',(4.7,-2.4,6.5));
#6569=CARTESIAN_POINT('',(4.7,-2.4,2.9));
#6570=CARTESIAN_POINT('Origin',(4.4,-2.,6.5));
#6571=CARTESIAN_POINT('Origin',(4.4,-2.,2.9));
#6572=CARTESIAN_POINT('',(4.7,-1.6,2.9));
#6573=CARTESIAN_POINT('',(2.7,-2.4,2.9));
#6574=CARTESIAN_POINT('',(4.125,-2.,2.9));
#6575=CARTESIAN_POINT('Origin',(4.4,-2.,2.9));
#6576=CARTESIAN_POINT('Origin',(1.,-2.4,2.));
#6577=CARTESIAN_POINT('',(1.,-2.4,6.5));
#6578=CARTESIAN_POINT('',(1.,-2.4,6.5));
#6579=CARTESIAN_POINT('',(1.,-2.4,2.8));
#6580=CARTESIAN_POINT('',(1.,-2.4,2.));
#6581=CARTESIAN_POINT('',(5.,-2.4,2.8));
#6582=CARTESIAN_POINT('',(1.,-2.4,2.8));
#6583=CARTESIAN_POINT('',(5.,-2.4,6.5));
#6584=CARTESIAN_POINT('',(5.,-2.4,2.));
#6585=CARTESIAN_POINT('',(1.,-2.4,6.5));
#6586=CARTESIAN_POINT('',(1.,-2.4,6.5));
#6587=CARTESIAN_POINT('',(2.495,-2.4,4.5));
#6588=CARTESIAN_POINT('Origin',(3.,-2.4,4.5));
#6589=CARTESIAN_POINT('Origin',(3.,-2.,6.5));
#6590=CARTESIAN_POINT('',(5.,-1.6,6.5));
#6591=CARTESIAN_POINT('',(5.,-2.4,6.5));
#6592=CARTESIAN_POINT('',(5.,-1.6,6.5));
#6593=CARTESIAN_POINT('Origin',(3.,-2.,6.5));
#6594=CARTESIAN_POINT('',(1.,-1.6,6.5));
#6595=CARTESIAN_POINT('',(5.,-1.6,6.5));
#6596=CARTESIAN_POINT('',(1.,-1.6,6.5));
#6597=CARTESIAN_POINT('Origin',(3.,-2.,6.5));
#6598=CARTESIAN_POINT('',(5.,-1.6,6.5));
#6599=CARTESIAN_POINT('Origin',(1.6,-2.,1.9));
#6600=CARTESIAN_POINT('',(1.325,-2.,2.));
#6601=CARTESIAN_POINT('Origin',(1.6,-2.,2.));
#6602=CARTESIAN_POINT('',(1.325,-2.,1.9));
#6603=CARTESIAN_POINT('Origin',(4.4,-2.,1.9));
#6604=CARTESIAN_POINT('',(4.125,-2.,2.));
#6605=CARTESIAN_POINT('Origin',(4.4,-2.,2.));
#6606=CARTESIAN_POINT('',(4.125,-2.,1.9));
#6607=CARTESIAN_POINT('Origin',(3.,-2.5,4.5));
#6608=CARTESIAN_POINT('',(2.495,-1.6,4.5));
#6609=CARTESIAN_POINT('',(2.495,-2.5,4.5));
#6610=CARTESIAN_POINT('Origin',(3.,-1.6,4.5));
#6611=CARTESIAN_POINT('Origin',(1.,-3.,2.8));
#6612=CARTESIAN_POINT('',(1.,-3.,2.8));
#6613=CARTESIAN_POINT('',(1.,-3.,2.8));
#6614=CARTESIAN_POINT('',(5.,-3.,2.8));
#6615=CARTESIAN_POINT('',(5.,-3.,2.8));
#6616=CARTESIAN_POINT('',(5.,-3.,2.8));
#6617=CARTESIAN_POINT('Origin',(1.,-3.,2.8));
#6618=CARTESIAN_POINT('',(5.,-1.6,2.8));
#6619=CARTESIAN_POINT('',(1.,-1.6,2.8));
#6620=CARTESIAN_POINT('',(3.,-1.6,2.8));
#6621=CARTESIAN_POINT('',(5.,-1.,2.8));
#6622=CARTESIAN_POINT('',(5.,-3.,2.8));
#6623=CARTESIAN_POINT('',(1.,-1.,2.8));
#6624=CARTESIAN_POINT('',(5.,-1.,2.8));
#6625=CARTESIAN_POINT('',(1.,-3.,2.8));
#6626=CARTESIAN_POINT('Origin',(3.,-1.,2.4));
#6627=CARTESIAN_POINT('',(5.,-1.,2.));
#6628=CARTESIAN_POINT('',(5.,-1.,2.));
#6629=CARTESIAN_POINT('',(1.,-1.,2.));
#6630=CARTESIAN_POINT('',(1.,-1.,2.));
#6631=CARTESIAN_POINT('',(1.,-1.,2.8));
#6632=CARTESIAN_POINT('Origin',(3.,-3.,2.4));
#6633=CARTESIAN_POINT('',(1.,-3.,2.));
#6634=CARTESIAN_POINT('',(1.,-3.,2.8));
#6635=CARTESIAN_POINT('',(5.,-3.,2.));
#6636=CARTESIAN_POINT('',(1.,-3.,2.));
#6637=CARTESIAN_POINT('',(5.,-3.,2.));
#6638=CARTESIAN_POINT('Origin',(5.,-1.6,2.));
#6639=CARTESIAN_POINT('',(5.,-1.6,2.));
#6640=CARTESIAN_POINT('',(1.,-1.6,2.));
#6641=CARTESIAN_POINT('Origin',(1.,-1.6,2.));
#6642=CARTESIAN_POINT('',(1.,-1.6,2.));
#6643=CARTESIAN_POINT('Origin',(5.,-2.4,2.));
#6644=CARTESIAN_POINT('',(5.,-3.,2.));
#6645=CARTESIAN_POINT('Origin',(3.,-2.,2.));
#6646=CARTESIAN_POINT('',(0.,0.,0.));
#6647=CARTESIAN_POINT('Origin',(1.6,32.,2.9));
#6648=CARTESIAN_POINT('',(1.3,32.4,6.5));
#6649=CARTESIAN_POINT('',(1.3,32.4,2.9));
#6650=CARTESIAN_POINT('',(1.3,32.4,2.9));
#6651=CARTESIAN_POINT('',(1.3,31.6,6.5));
#6652=CARTESIAN_POINT('Origin',(1.6,32.,6.5));
#6653=CARTESIAN_POINT('',(1.3,31.6,2.9));
#6654=CARTESIAN_POINT('',(1.3,31.6,2.9));
#6655=CARTESIAN_POINT('Origin',(1.6,32.,2.9));
#6656=CARTESIAN_POINT('Origin',(1.6,32.,2.9));
#6657=CARTESIAN_POINT('',(1.9,32.4,2.9));
#6658=CARTESIAN_POINT('',(1.9,32.4,6.5));
#6659=CARTESIAN_POINT('',(1.9,32.4,2.9));
#6660=CARTESIAN_POINT('',(1.9,31.6,2.9));
#6661=CARTESIAN_POINT('Origin',(1.6,32.,2.9));
#6662=CARTESIAN_POINT('',(1.9,31.6,6.5));
#6663=CARTESIAN_POINT('',(1.9,31.6,2.9));
#6664=CARTESIAN_POINT('Origin',(1.6,32.,6.5));
#6665=CARTESIAN_POINT('Origin',(1.6,32.,2.9));
#6666=CARTESIAN_POINT('',(3.3,32.4,2.9));
#6667=CARTESIAN_POINT('',(1.3,31.6,2.9));
#6668=CARTESIAN_POINT('',(1.325,32.,2.9));
#6669=CARTESIAN_POINT('Origin',(1.6,32.,2.9));
#6670=CARTESIAN_POINT('Origin',(4.4,32.,2.9));
#6671=CARTESIAN_POINT('',(4.1,32.4,6.5));
#6672=CARTESIAN_POINT('',(4.1,32.4,2.9));
#6673=CARTESIAN_POINT('',(4.1,32.4,2.9));
#6674=CARTESIAN_POINT('',(4.1,31.6,6.5));
#6675=CARTESIAN_POINT('Origin',(4.4,32.,6.5));
#6676=CARTESIAN_POINT('',(4.1,31.6,2.9));
#6677=CARTESIAN_POINT('',(4.1,31.6,2.9));
#6678=CARTESIAN_POINT('Origin',(4.4,32.,2.9));
#6679=CARTESIAN_POINT('Origin',(4.4,32.,2.9));
#6680=CARTESIAN_POINT('',(4.7,32.4,2.9));
#6681=CARTESIAN_POINT('',(4.7,32.4,6.5));
#6682=CARTESIAN_POINT('',(4.7,32.4,2.9));
#6683=CARTESIAN_POINT('',(4.7,31.6,2.9));
#6684=CARTESIAN_POINT('Origin',(4.4,32.,2.9));
#6685=CARTESIAN_POINT('',(4.7,31.6,6.5));
#6686=CARTESIAN_POINT('',(4.7,31.6,2.9));
#6687=CARTESIAN_POINT('Origin',(4.4,32.,6.5));
#6688=CARTESIAN_POINT('Origin',(4.4,32.,2.9));
#6689=CARTESIAN_POINT('',(4.7,32.4,2.9));
#6690=CARTESIAN_POINT('',(2.7,31.6,2.9));
#6691=CARTESIAN_POINT('',(4.125,32.,2.9));
#6692=CARTESIAN_POINT('Origin',(4.4,32.,2.9));
#6693=CARTESIAN_POINT('Origin',(1.,31.6,2.));
#6694=CARTESIAN_POINT('',(1.,31.6,6.5));
#6695=CARTESIAN_POINT('',(1.,31.6,6.5));
#6696=CARTESIAN_POINT('',(1.,31.6,2.8));
#6697=CARTESIAN_POINT('',(1.,31.6,2.));
#6698=CARTESIAN_POINT('',(5.,31.6,2.8));
#6699=CARTESIAN_POINT('',(1.,31.6,2.8));
#6700=CARTESIAN_POINT('',(5.,31.6,6.5));
#6701=CARTESIAN_POINT('',(5.,31.6,2.));
#6702=CARTESIAN_POINT('',(1.,31.6,6.5));
#6703=CARTESIAN_POINT('',(1.,31.6,6.5));
#6704=CARTESIAN_POINT('',(2.495,31.6,4.5));
#6705=CARTESIAN_POINT('Origin',(3.,31.6,4.5));
#6706=CARTESIAN_POINT('Origin',(3.,32.,6.5));
#6707=CARTESIAN_POINT('',(5.,32.4,6.5));
#6708=CARTESIAN_POINT('',(5.,31.6,6.5));
#6709=CARTESIAN_POINT('',(5.,32.4,6.5));
#6710=CARTESIAN_POINT('Origin',(3.,32.,6.5));
#6711=CARTESIAN_POINT('',(1.,32.4,6.5));
#6712=CARTESIAN_POINT('',(5.,32.4,6.5));
#6713=CARTESIAN_POINT('',(1.,32.4,6.5));
#6714=CARTESIAN_POINT('Origin',(3.,32.,6.5));
#6715=CARTESIAN_POINT('',(5.,32.4,6.5));
#6716=CARTESIAN_POINT('Origin',(1.6,32.,1.9));
#6717=CARTESIAN_POINT('',(1.325,32.,2.));
#6718=CARTESIAN_POINT('Origin',(1.6,32.,2.));
#6719=CARTESIAN_POINT('',(1.325,32.,1.9));
#6720=CARTESIAN_POINT('Origin',(4.4,32.,1.9));
#6721=CARTESIAN_POINT('',(4.125,32.,2.));
#6722=CARTESIAN_POINT('Origin',(4.4,32.,2.));
#6723=CARTESIAN_POINT('',(4.125,32.,1.9));
#6724=CARTESIAN_POINT('Origin',(3.,31.5,4.5));
#6725=CARTESIAN_POINT('',(2.495,32.4,4.5));
#6726=CARTESIAN_POINT('',(2.495,31.5,4.5));
#6727=CARTESIAN_POINT('Origin',(3.,32.4,4.5));
#6728=CARTESIAN_POINT('Origin',(1.,31.,2.8));
#6729=CARTESIAN_POINT('',(1.,31.,2.8));
#6730=CARTESIAN_POINT('',(1.,31.,2.8));
#6731=CARTESIAN_POINT('',(5.,31.,2.8));
#6732=CARTESIAN_POINT('',(5.,31.,2.8));
#6733=CARTESIAN_POINT('',(5.,31.,2.8));
#6734=CARTESIAN_POINT('Origin',(1.,31.,2.8));
#6735=CARTESIAN_POINT('',(5.,32.4,2.8));
#6736=CARTESIAN_POINT('',(1.,32.4,2.8));
#6737=CARTESIAN_POINT('',(3.,32.4,2.8));
#6738=CARTESIAN_POINT('',(5.,33.,2.8));
#6739=CARTESIAN_POINT('',(5.,31.,2.8));
#6740=CARTESIAN_POINT('',(1.,33.,2.8));
#6741=CARTESIAN_POINT('',(5.,33.,2.8));
#6742=CARTESIAN_POINT('',(1.,31.,2.8));
#6743=CARTESIAN_POINT('Origin',(3.,33.,2.4));
#6744=CARTESIAN_POINT('',(5.,33.,2.));
#6745=CARTESIAN_POINT('',(5.,33.,2.));
#6746=CARTESIAN_POINT('',(1.,33.,2.));
#6747=CARTESIAN_POINT('',(1.,33.,2.));
#6748=CARTESIAN_POINT('',(1.,33.,2.8));
#6749=CARTESIAN_POINT('Origin',(3.,31.,2.4));
#6750=CARTESIAN_POINT('',(1.,31.,2.));
#6751=CARTESIAN_POINT('',(1.,31.,2.8));
#6752=CARTESIAN_POINT('',(5.,31.,2.));
#6753=CARTESIAN_POINT('',(1.,31.,2.));
#6754=CARTESIAN_POINT('',(5.,31.,2.));
#6755=CARTESIAN_POINT('Origin',(5.,32.4,2.));
#6756=CARTESIAN_POINT('',(5.,32.4,2.));
#6757=CARTESIAN_POINT('',(1.,32.4,2.));
#6758=CARTESIAN_POINT('Origin',(1.,32.4,2.));
#6759=CARTESIAN_POINT('',(1.,32.4,2.));
#6760=CARTESIAN_POINT('Origin',(5.,31.6,2.));
#6761=CARTESIAN_POINT('',(5.,31.,2.));
#6762=CARTESIAN_POINT('Origin',(3.,32.,2.));
#6763=CARTESIAN_POINT('',(0.,0.,0.));
#6764=CARTESIAN_POINT('Origin',(0.115470053837925,-0.5,-0.2));
#6765=CARTESIAN_POINT('',(0.23094010767585,-0.5,0.));
#6766=CARTESIAN_POINT('',(0.115470053837925,-0.5,-0.2));
#6767=CARTESIAN_POINT('',(0.23094010767585,-0.5,0.));
#6768=CARTESIAN_POINT('',(0.115470053837925,-0.8,-0.2));
#6769=CARTESIAN_POINT('',(0.115470053837925,-0.5,-0.2));
#6770=CARTESIAN_POINT('',(0.23094010767585,-0.8,0.));
#6771=CARTESIAN_POINT('',(0.23094010767585,-0.8,0.));
#6772=CARTESIAN_POINT('',(0.23094010767585,-0.5,0.));
#6773=CARTESIAN_POINT('Origin',(-0.115470053837925,-0.5,-0.2));
#6774=CARTESIAN_POINT('',(-0.115470053837925,-0.5,-0.2));
#6775=CARTESIAN_POINT('',(0.115470053837925,-0.5,-0.2));
#6776=CARTESIAN_POINT('',(-0.115470053837925,-0.8,-0.2));
#6777=CARTESIAN_POINT('',(-0.115470053837925,-0.5,-0.2));
#6778=CARTESIAN_POINT('',(0.115470053837925,-0.8,-0.2));
#6779=CARTESIAN_POINT('Origin',(-0.23094010767585,-0.5,-2.77555756156289E-17));
#6780=CARTESIAN_POINT('',(-0.23094010767585,-0.5,-2.82820063659975E-17));
#6781=CARTESIAN_POINT('',(-0.115470053837925,-0.5,-0.2));
#6782=CARTESIAN_POINT('',(-0.23094010767585,-0.8,-2.77555756156289E-17));
#6783=CARTESIAN_POINT('',(-0.23094010767585,-0.5,-2.82820063659975E-17));
#6784=CARTESIAN_POINT('',(-0.115470053837925,-0.8,-0.2));
#6785=CARTESIAN_POINT('Origin',(-0.115470053837925,-0.5,0.2));
#6786=CARTESIAN_POINT('',(-0.115470053837925,-0.5,0.2));
#6787=CARTESIAN_POINT('',(-0.23094010767585,-0.5,-2.82820063659975E-17));
#6788=CARTESIAN_POINT('',(-0.115470053837925,-0.8,0.2));
#6789=CARTESIAN_POINT('',(-0.115470053837925,-0.5,0.2));
#6790=CARTESIAN_POINT('',(-0.23094010767585,-0.8,-2.82820063659975E-17));
#6791=CARTESIAN_POINT('Origin',(0.115470053837925,-0.5,0.2));
#6792=CARTESIAN_POINT('',(0.115470053837925,-0.5,0.2));
#6793=CARTESIAN_POINT('',(-0.115470053837925,-0.5,0.2));
#6794=CARTESIAN_POINT('',(0.115470053837925,-0.8,0.2));
#6795=CARTESIAN_POINT('',(0.115470053837925,-0.5,0.2));
#6796=CARTESIAN_POINT('',(-0.115470053837925,-0.8,0.2));
#6797=CARTESIAN_POINT('Origin',(0.23094010767585,-0.5,0.));
#6798=CARTESIAN_POINT('',(0.115470053837925,-0.5,0.2));
#6799=CARTESIAN_POINT('',(0.115470053837925,-0.8,0.2));
#6800=CARTESIAN_POINT('Origin',(0.,-0.5,0.));
#6801=CARTESIAN_POINT('Origin',(0.,-0.8,0.));
#6802=CARTESIAN_POINT('Origin',(0.,-1.4,0.));
#6803=CARTESIAN_POINT('',(-0.24505,-1.4,3.00099698131059E-17));
#6804=CARTESIAN_POINT('Origin',(0.,-1.4,0.));
#6805=CARTESIAN_POINT('Origin',(0.375,0.5,0.));
#6806=CARTESIAN_POINT('',(-0.375,0.5,-4.59242549680257E-17));
#6807=CARTESIAN_POINT('Origin',(0.,0.5,0.));
#6808=CARTESIAN_POINT('Origin',(0.,0.475,0.));
#6809=CARTESIAN_POINT('',(-0.425,0.45,-5.20474889637625E-17));
#6810=CARTESIAN_POINT('Origin',(0.,0.45,0.));
#6811=CARTESIAN_POINT('',(-0.4,0.475,-4.89858719658941E-17));
#6812=CARTESIAN_POINT('Origin',(0.,0.24,0.));
#6813=CARTESIAN_POINT('',(-0.425,0.0299999999999998,-5.20474889637625E-17));
#6814=CARTESIAN_POINT('Origin',(0.,0.0299999999999998,0.));
#6815=CARTESIAN_POINT('',(-0.425,0.24,-5.20474889637625E-17));
#6816=CARTESIAN_POINT('Origin',(0.,0.0150000000000001,0.));
#6817=CARTESIAN_POINT('',(-0.395,4.85722573273506E-17,-4.83735485663204E-17));
#6818=CARTESIAN_POINT('Origin',(0.,0.,0.));
#6819=CARTESIAN_POINT('',(-0.41,0.0150000000000001,-5.02105187650415E-17));
#6820=CARTESIAN_POINT('Origin',(0.27,0.,0.));
#6821=CARTESIAN_POINT('',(-0.27,0.,-3.30654635769785E-17));
#6822=CARTESIAN_POINT('Origin',(0.,0.,0.));
#6823=CARTESIAN_POINT('Origin',(0.,-0.02,0.));
#6824=CARTESIAN_POINT('',(-0.24505,-0.0498999999999999,3.00099698131059E-17));
#6825=CARTESIAN_POINT('Origin',(0.,-0.0498999999999999,0.));
#6826=CARTESIAN_POINT('',(-0.26,-0.02,-3.18408167778312E-17));
#6827=CARTESIAN_POINT('Origin',(0.,-0.995,0.));
#6828=CARTESIAN_POINT('',(-0.24505,-0.995,-3.00099698131059E-17));
#6829=CARTESIAN_POINT('',(0.,0.,0.));
#6830=CARTESIAN_POINT('Origin',(0.,0.395,0.25));
#6831=CARTESIAN_POINT('',(-0.5,0.3,0.25));
#6832=CARTESIAN_POINT('',(0.5,0.3,0.25));
#6833=CARTESIAN_POINT('',(0.25,0.3,0.25));
#6834=CARTESIAN_POINT('',(-0.5,0.5,0.25));
#6835=CARTESIAN_POINT('',(-0.5,0.5,0.25));
#6836=CARTESIAN_POINT('',(0.5,0.5,0.25));
#6837=CARTESIAN_POINT('',(0.5,0.5,0.25));
#6838=CARTESIAN_POINT('',(0.5,0.29,0.25));
#6839=CARTESIAN_POINT('Origin',(0.5,0.5,0.25));
#6840=CARTESIAN_POINT('',(-0.5,0.5,0.4));
#6841=CARTESIAN_POINT('',(-0.5,0.5,0.25));
#6842=CARTESIAN_POINT('',(0.5,0.5,0.4));
#6843=CARTESIAN_POINT('',(0.5,0.5,0.4));
#6844=CARTESIAN_POINT('',(0.5,0.5,0.25));
#6845=CARTESIAN_POINT('Origin',(0.,0.,0.4));
#6846=CARTESIAN_POINT('',(-0.5,-0.5,0.4));
#6847=CARTESIAN_POINT('',(-0.5,0.5,0.4));
#6848=CARTESIAN_POINT('',(0.5,-0.5,0.4));
#6849=CARTESIAN_POINT('',(-0.5,-0.5,0.4));
#6850=CARTESIAN_POINT('',(0.5,-0.3,0.4));
#6851=CARTESIAN_POINT('',(-0.2117,2.59257727379495E-17,0.4));
#6852=CARTESIAN_POINT('Origin',(0.,0.,0.4));
#6853=CARTESIAN_POINT('Origin',(-0.5,0.3,0.));
#6854=CARTESIAN_POINT('',(-0.5,0.3,0.15));
#6855=CARTESIAN_POINT('',(-0.5,0.3,0.));
#6856=CARTESIAN_POINT('',(-0.5,0.15,0.));
#6857=CARTESIAN_POINT('',(-0.5,0.225,0.075));
#6858=CARTESIAN_POINT('',(-0.5,-0.15,0.));
#6859=CARTESIAN_POINT('',(-0.5,0.3,0.));
#6860=CARTESIAN_POINT('',(-0.5,-0.3,0.15));
#6861=CARTESIAN_POINT('',(-0.5,-0.075,-0.075));
#6862=CARTESIAN_POINT('',(-0.5,-0.3,0.25));
#6863=CARTESIAN_POINT('',(-0.5,-0.3,0.));
#6864=CARTESIAN_POINT('',(-0.5,-0.5,0.25));
#6865=CARTESIAN_POINT('',(-0.5,-0.29,0.25));
#6866=CARTESIAN_POINT('',(-0.5,-0.5,0.25));
#6867=CARTESIAN_POINT('Origin',(-0.5,-0.5,0.25));
#6868=CARTESIAN_POINT('',(0.5,-0.5,0.25));
#6869=CARTESIAN_POINT('',(-0.5,-0.5,0.25));
#6870=CARTESIAN_POINT('',(0.5,-0.5,0.25));
#6871=CARTESIAN_POINT('Origin',(0.,-0.395,0.25));
#6872=CARTESIAN_POINT('',(0.5,-0.3,0.25));
#6873=CARTESIAN_POINT('',(-0.25,-0.3,0.25));
#6874=CARTESIAN_POINT('',(0.5,-0.5,0.25));
#6875=CARTESIAN_POINT('Origin',(0.5,-0.3,0.));
#6876=CARTESIAN_POINT('',(0.5,-0.3,0.15));
#6877=CARTESIAN_POINT('',(0.5,-0.3,0.));
#6878=CARTESIAN_POINT('',(0.5,-0.15,0.));
#6879=CARTESIAN_POINT('',(0.5,-0.225,0.075));
#6880=CARTESIAN_POINT('',(0.5,0.15,0.));
#6881=CARTESIAN_POINT('',(0.5,-0.3,0.));
#6882=CARTESIAN_POINT('',(0.5,0.3,0.15));
#6883=CARTESIAN_POINT('',(0.5,0.075,-0.075));
#6884=CARTESIAN_POINT('',(0.5,0.3,0.));
#6885=CARTESIAN_POINT('Origin',(-0.5,-0.3,0.));
#6886=CARTESIAN_POINT('',(-0.25,-0.3,0.15));
#6887=CARTESIAN_POINT('Origin',(-0.25,-0.225,0.075));
#6888=CARTESIAN_POINT('',(-0.149388386429468,-0.15,0.));
#6889=CARTESIAN_POINT('',(-0.25,-0.15,0.));
#6890=CARTESIAN_POINT('',(0.149388386429468,-0.15,0.));
#6891=CARTESIAN_POINT('Origin',(0.,0.,-0.15));
#6892=CARTESIAN_POINT('',(-0.25,-0.15,0.));
#6893=CARTESIAN_POINT('Origin',(0.,0.,-0.1));
#6894=CARTESIAN_POINT('',(-0.2117,-2.59257727379495E-17,0.));
#6895=CARTESIAN_POINT('Origin',(0.,0.,0.));
#6896=CARTESIAN_POINT('',(-0.2117,-2.59257727379495E-17,-0.1));
#6897=CARTESIAN_POINT('',(-0.149388386429468,0.15,0.));
#6898=CARTESIAN_POINT('Origin',(0.,0.,0.));
#6899=CARTESIAN_POINT('',(0.149388386429468,0.15,0.));
#6900=CARTESIAN_POINT('Origin',(0.,0.,-0.15));
#6901=CARTESIAN_POINT('Origin',(0.,0.,0.));
#6902=CARTESIAN_POINT('Origin',(0.,0.,0.));
#6903=CARTESIAN_POINT('',(0.25,0.15,0.));
#6904=CARTESIAN_POINT('Origin',(0.,0.,0.));
#6905=CARTESIAN_POINT('',(0.25,0.15,0.));
#6906=CARTESIAN_POINT('Origin',(0.25,0.225,0.075));
#6907=CARTESIAN_POINT('',(0.25,0.3,0.15));
#6908=CARTESIAN_POINT('Origin',(0.5,0.3,0.));
#6909=CARTESIAN_POINT('',(0.,0.,0.));
#6910=CARTESIAN_POINT('',(0.,0.,0.));
#6911=CARTESIAN_POINT('Origin',(0.,0.,0.));
#6912=CARTESIAN_POINT('',(-0.976185,-0.246528389340863,-1.19548183562566E-16));
#6913=CARTESIAN_POINT('',(-1.19548183562566E-16,-0.246528389340863,0.976185));
#6914=CARTESIAN_POINT('Origin',(0.,-0.246528389340863,0.));
#6915=CARTESIAN_POINT('Origin',(0.,-0.246528389340863,0.));
#6916=CARTESIAN_POINT('',(-1.19548183562566E-16,0.246528389340863,0.976185));
#6917=CARTESIAN_POINT('Origin',(-1.22464679914735E-16,0.,1.));
#6918=CARTESIAN_POINT('',(-0.976185,0.246528389340863,1.19548183562566E-16));
#6919=CARTESIAN_POINT('Origin',(0.,0.246528389340863,0.));
#6920=CARTESIAN_POINT('Origin',(0.,0.246528389340863,0.));
#6921=CARTESIAN_POINT('Origin',(0.,0.,0.));
#6922=CARTESIAN_POINT('',(-0.976185,0.45,-1.19548183562566E-16));
#6923=CARTESIAN_POINT('',(-0.976185,0.,-1.19548183562566E-16));
#6924=CARTESIAN_POINT('Origin',(0.,0.45,0.));
#6925=CARTESIAN_POINT('Origin',(0.,0.,0.));
#6926=CARTESIAN_POINT('',(-0.5,-0.39,-6.12323399573677E-17));
#6927=CARTESIAN_POINT('Origin',(0.,-0.39,0.));
#6928=CARTESIAN_POINT('',(-0.5,0.39,-6.12323399573677E-17));
#6929=CARTESIAN_POINT('',(-0.5,0.,-6.12323399573677E-17));
#6930=CARTESIAN_POINT('Origin',(0.,0.39,0.));
#6931=CARTESIAN_POINT('Origin',(0.,0.42,0.));
#6932=CARTESIAN_POINT('',(-0.56,0.45,-6.85802207522518E-17));
#6933=CARTESIAN_POINT('',(-0.53,0.42,-6.49062803548097E-17));
#6934=CARTESIAN_POINT('Origin',(0.,0.45,0.));
#6935=CARTESIAN_POINT('Origin',(0.976185,0.45,0.));
#6936=CARTESIAN_POINT('Origin',(0.,0.,0.));
#6937=CARTESIAN_POINT('',(-0.976185,-0.45,-1.19548183562566E-16));
#6938=CARTESIAN_POINT('Origin',(0.,-0.45,0.));
#6939=CARTESIAN_POINT('',(-0.976185,0.,-1.19548183562566E-16));
#6940=CARTESIAN_POINT('Origin',(0.56,-0.45,0.));
#6941=CARTESIAN_POINT('',(-0.56,-0.45,-6.85802207522518E-17));
#6942=CARTESIAN_POINT('Origin',(0.,-0.45,0.));
#6943=CARTESIAN_POINT('Origin',(0.,-0.42,0.));
#6944=CARTESIAN_POINT('',(-0.53,-0.42,-6.49062803548097E-17));
#6945=CARTESIAN_POINT('',(0.,0.,0.));
#6946=CARTESIAN_POINT('Origin',(0.,0.,0.));
#6947=CARTESIAN_POINT('',(-1.023815,0.246528389340863,-1.25381176266905E-16));
#6948=CARTESIAN_POINT('',(-1.25381176266905E-16,0.246528389340863,1.023815));
#6949=CARTESIAN_POINT('Origin',(0.,0.246528389340863,0.));
#6950=CARTESIAN_POINT('Origin',(0.,0.246528389340863,0.));
#6951=CARTESIAN_POINT('',(-1.25381176266905E-16,-0.246528389340863,1.023815));
#6952=CARTESIAN_POINT('Origin',(-1.22464679914735E-16,0.,1.));
#6953=CARTESIAN_POINT('',(-1.023815,-0.246528389340863,1.25381176266905E-16));
#6954=CARTESIAN_POINT('Origin',(0.,-0.246528389340863,0.));
#6955=CARTESIAN_POINT('Origin',(0.,-0.246528389340863,0.));
#6956=CARTESIAN_POINT('Origin',(0.,0.,0.));
#6957=CARTESIAN_POINT('',(-1.023815,-0.45,-1.25381176266905E-16));
#6958=CARTESIAN_POINT('Origin',(0.,-0.45,0.));
#6959=CARTESIAN_POINT('',(-1.023815,0.,-1.25381176266905E-16));
#6960=CARTESIAN_POINT('Origin',(1.44,0.45,0.));
#6961=CARTESIAN_POINT('',(-1.44,0.45,-1.76349139077219E-16));
#6962=CARTESIAN_POINT('Origin',(0.,0.45,0.));
#6963=CARTESIAN_POINT('',(-1.023815,0.45,-1.25381176266905E-16));
#6964=CARTESIAN_POINT('Origin',(0.,0.45,0.));
#6965=CARTESIAN_POINT('Origin',(0.,0.42,0.));
#6966=CARTESIAN_POINT('',(-1.5,0.39,-1.83697019872103E-16));
#6967=CARTESIAN_POINT('Origin',(0.,0.39,0.));
#6968=CARTESIAN_POINT('',(-1.47,0.42,-1.80023079474661E-16));
#6969=CARTESIAN_POINT('Origin',(0.,0.,0.));
#6970=CARTESIAN_POINT('',(-1.5,-0.39,-1.83697019872103E-16));
#6971=CARTESIAN_POINT('Origin',(0.,-0.39,0.));
#6972=CARTESIAN_POINT('',(-1.5,0.,-1.83697019872103E-16));
#6973=CARTESIAN_POINT('Origin',(0.,-0.42,0.));
#6974=CARTESIAN_POINT('',(-1.44,-0.45,-1.76349139077219E-16));
#6975=CARTESIAN_POINT('Origin',(0.,-0.45,0.));
#6976=CARTESIAN_POINT('',(-1.47,-0.42,-1.80023079474661E-16));
#6977=CARTESIAN_POINT('Origin',(1.023815,-0.45,0.));
#6978=CARTESIAN_POINT('Origin',(0.,0.,0.));
#6979=CARTESIAN_POINT('',(-1.023815,0.,-1.25381176266905E-16));
#6980=CARTESIAN_POINT('',(0.,0.,0.));
#6981=CARTESIAN_POINT('Origin',(1.,0.,0.));
#6982=CARTESIAN_POINT('',(1.,-1.78583896120461E-33,0.23815));
#6983=CARTESIAN_POINT('',(1.,-1.78583896120461E-33,-0.23815));
#6984=CARTESIAN_POINT('Origin',(1.,0.,0.));
#6985=CARTESIAN_POINT('Origin',(0.707106781186548,0.,-0.707106781186547));
#6986=CARTESIAN_POINT('',(0.875504261126124,-1.78583896120461E-33,-0.538709301246971));
#6987=CARTESIAN_POINT('',(0.538709301246971,-1.78583896120461E-33,-0.875504261126124));
#6988=CARTESIAN_POINT('Origin',(0.707106781186548,0.,-0.707106781186547));
#6989=CARTESIAN_POINT('Origin',(6.12323399573677E-17,0.,-1.));
#6990=CARTESIAN_POINT('',(0.23815,-1.78583896120461E-33,-1.));
#6991=CARTESIAN_POINT('',(-0.23815,-1.78583896120461E-33,-1.));
#6992=CARTESIAN_POINT('Origin',(6.12323399573677E-17,0.,-1.));
#6993=CARTESIAN_POINT('Origin',(-0.707106781186547,0.,-0.707106781186548));
#6994=CARTESIAN_POINT('',(-0.538709301246971,-1.78583896120461E-33,-0.875504261126124));
#6995=CARTESIAN_POINT('',(-0.875504261126124,-1.78583896120461E-33,-0.538709301246971));
#6996=CARTESIAN_POINT('Origin',(-0.707106781186547,0.,-0.707106781186548));
#6997=CARTESIAN_POINT('Origin',(-1.,0.,-1.22464679914735E-16));
#6998=CARTESIAN_POINT('',(-1.,-1.78583896120461E-33,-0.23815));
#6999=CARTESIAN_POINT('',(-1.,-1.78583896120461E-33,0.23815));
#7000=CARTESIAN_POINT('Origin',(-1.,0.,-1.22464679914735E-16));
#7001=CARTESIAN_POINT('Origin',(-0.707106781186548,0.,0.707106781186547));
#7002=CARTESIAN_POINT('',(-0.875504261126124,-7.94881478324376E-33,0.538709301246971));
#7003=CARTESIAN_POINT('',(-0.538709301246971,4.37713686083455E-33,0.875504261126124));
#7004=CARTESIAN_POINT('Origin',(-0.707106781186548,0.,0.707106781186547));
#7005=CARTESIAN_POINT('Origin',(-1.83697019872103E-16,0.,1.));
#7006=CARTESIAN_POINT('',(-0.23815,-1.78583896120461E-33,1.));
#7007=CARTESIAN_POINT('',(0.23815,-1.78583896120461E-33,1.));
#7008=CARTESIAN_POINT('Origin',(-1.83697019872103E-16,0.,1.));
#7009=CARTESIAN_POINT('Origin',(0.707106781186547,0.,0.707106781186548));
#7010=CARTESIAN_POINT('',(0.538709301246971,-4.86732687222419E-33,0.875504261126124));
#7011=CARTESIAN_POINT('',(0.875504261126124,1.29564894981497E-33,0.538709301246971));
#7012=CARTESIAN_POINT('Origin',(0.707106781186547,0.,0.707106781186548));
#7013=CARTESIAN_POINT('',(0.,0.,0.));
#7014=CARTESIAN_POINT('Origin',(0.707106781186547,0.,0.707106781186548));
#7015=CARTESIAN_POINT('',(0.504455939115715,-0.04763,0.841298510752802));
#7016=CARTESIAN_POINT('',(0.841298510752802,-0.04763,0.504455939115715));
#7017=CARTESIAN_POINT('Ctrl Pts',(0.504455939115715,-0.04763,0.841298510752802));
#7018=CARTESIAN_POINT('Ctrl Pts',(0.508899795931835,-0.0740444353928835,
0.838633903678357));
#7019=CARTESIAN_POINT('Ctrl Pts',(0.517157748491652,-0.0999305678883309,
0.833661031856294));
#7020=CARTESIAN_POINT('Ctrl Pts',(0.537715343527944,-0.142345102874864,
0.820511285096538));
#7021=CARTESIAN_POINT('Ctrl Pts',(0.548874290046456,-0.159766064500479,
0.813159949759));
#7022=CARTESIAN_POINT('Ctrl Pts',(0.573915184558107,-0.190326085855194,
0.795684265985089));
#7023=CARTESIAN_POINT('Ctrl Pts',(0.587792702767295,-0.203463743702801,
0.78555112003688));
#7024=CARTESIAN_POINT('Ctrl Pts',(0.615966552324775,-0.224161999508995,
0.763642258217233));
#7025=CARTESIAN_POINT('Ctrl Pts',(0.631684198665438,-0.232861760990032,
0.750785745543687));
#7026=CARTESIAN_POINT('Ctrl Pts',(0.663382628119203,-0.244251601209411,
0.722929908501543));
#7027=CARTESIAN_POINT('Ctrl Pts',(0.679352081686668,-0.246942143572133,
0.707917883896095));
#7028=CARTESIAN_POINT('Ctrl Pts',(0.707917883896095,-0.246942143572133,
0.679352081686668));
#7029=CARTESIAN_POINT('Ctrl Pts',(0.722929908501543,-0.244251601209411,
0.663382628119203));
#7030=CARTESIAN_POINT('Ctrl Pts',(0.750785745543687,-0.232861760990032,
0.631684198665439));
#7031=CARTESIAN_POINT('Ctrl Pts',(0.763642258217232,-0.224161999508995,
0.615966552324775));
#7032=CARTESIAN_POINT('Ctrl Pts',(0.78555112003688,-0.203463743702801,0.587792702767295));
#7033=CARTESIAN_POINT('Ctrl Pts',(0.795684265985088,-0.190326085855194,
0.573915184558108));
#7034=CARTESIAN_POINT('Ctrl Pts',(0.813159949759,-0.15976606450048,0.548874290046456));
#7035=CARTESIAN_POINT('Ctrl Pts',(0.820511285096538,-0.142345102874864,
0.537715343527944));
#7036=CARTESIAN_POINT('Ctrl Pts',(0.833661031856294,-0.099930567888331,
0.517157748491653));
#7037=CARTESIAN_POINT('Ctrl Pts',(0.838633903678357,-0.0740444353928835,
0.508899795931835));
#7038=CARTESIAN_POINT('Ctrl Pts',(0.841298510752801,-0.0476299999999999,
0.504455939115715));
#7039=CARTESIAN_POINT('',(0.528110872004958,-0.04763,0.871530771444223));
#7040=CARTESIAN_POINT('Origin',(0.707106781186547,-0.04763,0.707106781186548));
#7041=CARTESIAN_POINT('',(0.871530771444223,-0.04763,0.528110872004959));
#7042=CARTESIAN_POINT('Ctrl Pts',(0.871530771444223,-0.0476300000000001,
0.528110872004958));
#7043=CARTESIAN_POINT('Ctrl Pts',(0.87014664509073,-0.0609922781173483,
0.530395067942936));
#7044=CARTESIAN_POINT('Ctrl Pts',(0.868149331745851,-0.0742967091364493,
0.533674141594226));
#7045=CARTESIAN_POINT('Ctrl Pts',(0.85981294420286,-0.115492077056649,0.54708917182331));
#7046=CARTESIAN_POINT('Ctrl Pts',(0.850993704737257,-0.141695629206859,
0.560922177770136));
#7047=CARTESIAN_POINT('Ctrl Pts',(0.830754510485543,-0.181890537957859,
0.590422647829571));
#7048=CARTESIAN_POINT('Ctrl Pts',(0.816896541396381,-0.201072148666545,
0.609616703125488));
#7049=CARTESIAN_POINT('Ctrl Pts',(0.792310597819928,-0.223955109275652,
0.641117951819998));
#7050=CARTESIAN_POINT('Ctrl Pts',(0.779109323683612,-0.232742381310829,
0.657208095763053));
#7051=CARTESIAN_POINT('Ctrl Pts',(0.750552691816206,-0.244234834628584,
0.68964083160521));
#7052=CARTESIAN_POINT('Ctrl Pts',(0.735185187071673,-0.246942143572133,
0.705971972091755));
#7053=CARTESIAN_POINT('Ctrl Pts',(0.705971972091754,-0.246942143572133,
0.735185187071673));
#7054=CARTESIAN_POINT('Ctrl Pts',(0.689640831605209,-0.244234834628584,
0.750552691816206));
#7055=CARTESIAN_POINT('Ctrl Pts',(0.657208095763052,-0.232742381310829,
0.779109323683612));
#7056=CARTESIAN_POINT('Ctrl Pts',(0.641117951819998,-0.223955109275652,
0.792310597819928));
#7057=CARTESIAN_POINT('Ctrl Pts',(0.609616703125487,-0.201072148666545,
0.816896541396382));
#7058=CARTESIAN_POINT('Ctrl Pts',(0.590422647829571,-0.181890537957858,
0.830754510485544));
#7059=CARTESIAN_POINT('Ctrl Pts',(0.560922177770135,-0.141695629206858,
0.850993704737257));
#7060=CARTESIAN_POINT('Ctrl Pts',(0.547089171823309,-0.115492077056649,
0.859812944202861));
#7061=CARTESIAN_POINT('Ctrl Pts',(0.533674141594226,-0.0742967091364491,
0.868149331745852));
#7062=CARTESIAN_POINT('Ctrl Pts',(0.530395067942936,-0.0609922781173483,
0.870146645090731));
#7063=CARTESIAN_POINT('Ctrl Pts',(0.528110872004958,-0.0476300000000001,
0.871530771444223));
#7064=CARTESIAN_POINT('Origin',(0.707106781186547,-0.04763,0.707106781186548));
#7065=CARTESIAN_POINT('Origin',(0.,-0.166705,0.));
#7066=CARTESIAN_POINT('',(0.242834539687906,-0.04763,0.989696097314));
#7067=CARTESIAN_POINT('Origin',(0.,-0.04763,0.));
#7068=CARTESIAN_POINT('',(-0.242834539687907,-0.04763,0.989696097314));
#7069=CARTESIAN_POINT('Ctrl Pts',(0.242834539687906,-0.04763,0.989696097314));
#7070=CARTESIAN_POINT('Ctrl Pts',(0.24024064412003,-0.0609922781173483,
0.990332542620729));
#7071=CARTESIAN_POINT('Ctrl Pts',(0.236509675094874,-0.0742967091364492,
0.991238884025248));
#7072=CARTESIAN_POINT('Ctrl Pts',(0.221129100087819,-0.115492077056649,
0.994830026707808));
#7073=CARTESIAN_POINT('Ctrl Pts',(0.205111543747588,-0.141695629206859,
0.998375294985966));
#7074=CARTESIAN_POINT('Ctrl Pts',(0.169940289819232,-0.181890537957859,
1.00492400591205));
#7075=CARTESIAN_POINT('Ctrl Pts',(0.1465689792446,-0.201072148666545,1.00869718865384));
#7076=CARTESIAN_POINT('Ctrl Pts',(0.106909345252087,-0.223955109275652,
1.01358704779679));
#7077=CARTESIAN_POINT('Ctrl Pts',(0.0861971848975941,-0.232742381310829,
1.0156297872271));
#7078=CARTESIAN_POINT('Ctrl Pts',(0.0430711894098822,-0.244234834628584,
1.01837060663223));
#7079=CARTESIAN_POINT('Ctrl Pts',(0.0206568624125605,-0.246942143572133,
1.019052));
#7080=CARTESIAN_POINT('Ctrl Pts',(-0.0206568624125608,-0.246942143572133,
1.019052));
#7081=CARTESIAN_POINT('Ctrl Pts',(-0.0430711894098825,-0.244234834628584,
1.01837060663223));
#7082=CARTESIAN_POINT('Ctrl Pts',(-0.0861971848975943,-0.232742381310829,
1.0156297872271));
#7083=CARTESIAN_POINT('Ctrl Pts',(-0.106909345252088,-0.223955109275652,
1.01358704779679));
#7084=CARTESIAN_POINT('Ctrl Pts',(-0.1465689792446,-0.201072148666545,1.00869718865384));
#7085=CARTESIAN_POINT('Ctrl Pts',(-0.169940289819232,-0.181890537957859,
1.00492400591205));
#7086=CARTESIAN_POINT('Ctrl Pts',(-0.205111543747588,-0.141695629206859,
0.998375294985966));
#7087=CARTESIAN_POINT('Ctrl Pts',(-0.221129100087819,-0.115492077056649,
0.994830026707808));
#7088=CARTESIAN_POINT('Ctrl Pts',(-0.236509675094875,-0.0742967091364493,
0.991238884025248));
#7089=CARTESIAN_POINT('Ctrl Pts',(-0.24024064412003,-0.0609922781173483,
0.990332542620729));
#7090=CARTESIAN_POINT('Ctrl Pts',(-0.242834539687907,-0.04763,0.989696097314));
#7091=CARTESIAN_POINT('',(-0.528110872004959,-0.04763,0.871530771444223));
#7092=CARTESIAN_POINT('Origin',(0.,-0.04763,0.));
#7093=CARTESIAN_POINT('',(-0.871530771444223,-0.04763,0.528110872004958));
#7094=CARTESIAN_POINT('Ctrl Pts',(-0.528110872004958,-0.0476300000000001,
0.871530771444223));
#7095=CARTESIAN_POINT('Ctrl Pts',(-0.530395067942936,-0.0609922781173484,
0.87014664509073));
#7096=CARTESIAN_POINT('Ctrl Pts',(-0.533674141594226,-0.0742967091364493,
0.868149331745851));
#7097=CARTESIAN_POINT('Ctrl Pts',(-0.54708917182331,-0.115492077056649,
0.85981294420286));
#7098=CARTESIAN_POINT('Ctrl Pts',(-0.560922177770136,-0.141695629206859,
0.850993704737257));
#7099=CARTESIAN_POINT('Ctrl Pts',(-0.590422647829571,-0.181890537957859,
0.830754510485543));
#7100=CARTESIAN_POINT('Ctrl Pts',(-0.609616703125488,-0.201072148666545,
0.816896541396381));
#7101=CARTESIAN_POINT('Ctrl Pts',(-0.641117951819998,-0.223955109275652,
0.792310597819928));
#7102=CARTESIAN_POINT('Ctrl Pts',(-0.657208095763053,-0.232742381310829,
0.779109323683611));
#7103=CARTESIAN_POINT('Ctrl Pts',(-0.68964083160521,-0.244234834628584,
0.750552691816205));
#7104=CARTESIAN_POINT('Ctrl Pts',(-0.705971972091755,-0.246942143572133,
0.735185187071673));
#7105=CARTESIAN_POINT('Ctrl Pts',(-0.735185187071673,-0.246942143572133,
0.705971972091754));
#7106=CARTESIAN_POINT('Ctrl Pts',(-0.750552691816206,-0.244234834628584,
0.689640831605209));
#7107=CARTESIAN_POINT('Ctrl Pts',(-0.779109323683612,-0.232742381310829,
0.657208095763052));
#7108=CARTESIAN_POINT('Ctrl Pts',(-0.792310597819928,-0.223955109275652,
0.641117951819998));
#7109=CARTESIAN_POINT('Ctrl Pts',(-0.816896541396382,-0.201072148666545,
0.609616703125487));
#7110=CARTESIAN_POINT('Ctrl Pts',(-0.830754510485544,-0.181890537957858,
0.590422647829571));
#7111=CARTESIAN_POINT('Ctrl Pts',(-0.850993704737257,-0.141695629206858,
0.560922177770135));
#7112=CARTESIAN_POINT('Ctrl Pts',(-0.859812944202861,-0.115492077056649,
0.547089171823309));
#7113=CARTESIAN_POINT('Ctrl Pts',(-0.868149331745852,-0.0742967091364491,
0.533674141594226));
#7114=CARTESIAN_POINT('Ctrl Pts',(-0.870146645090731,-0.0609922781173483,
0.530395067942936));
#7115=CARTESIAN_POINT('Ctrl Pts',(-0.871530771444223,-0.04763,0.528110872004958));
#7116=CARTESIAN_POINT('',(-0.989696097314,-0.04763,0.242834539687906));
#7117=CARTESIAN_POINT('Origin',(0.,-0.04763,0.));
#7118=CARTESIAN_POINT('',(-1.019052,-0.246942143572133,1.248489836334E-16));
#7119=CARTESIAN_POINT('Ctrl Pts',(-0.989696097314,-0.04763,0.242834539687906));
#7120=CARTESIAN_POINT('Ctrl Pts',(-0.990332542620729,-0.0609922781173483,
0.24024064412003));
#7121=CARTESIAN_POINT('Ctrl Pts',(-0.991238884025248,-0.0742967091364492,
0.236509675094874));
#7122=CARTESIAN_POINT('Ctrl Pts',(-0.994830026707808,-0.115492077056649,
0.221129100087819));
#7123=CARTESIAN_POINT('Ctrl Pts',(-0.998375294985966,-0.141695629206859,
0.205111543747588));
#7124=CARTESIAN_POINT('Ctrl Pts',(-1.00492400591205,-0.181890537957859,
0.169940289819232));
#7125=CARTESIAN_POINT('Ctrl Pts',(-1.00869718865384,-0.201072148666545,
0.1465689792446));
#7126=CARTESIAN_POINT('Ctrl Pts',(-1.01358704779679,-0.223955109275652,
0.106909345252088));
#7127=CARTESIAN_POINT('Ctrl Pts',(-1.0156297872271,-0.232742381310829,0.0861971848975944));
#7128=CARTESIAN_POINT('Ctrl Pts',(-1.01837060663223,-0.244234834628584,
0.0430711894098825));
#7129=CARTESIAN_POINT('Ctrl Pts',(-1.019052,-0.246942143572133,0.0206568624125608));
#7130=CARTESIAN_POINT('Ctrl Pts',(-1.019052,-0.246942143572133,1.2490009027033E-16));
#7131=CARTESIAN_POINT('',(-1.019052,-0.28578,1.24797876996471E-16));
#7132=CARTESIAN_POINT('',(-1.019052,-0.166705,1.24797876996471E-16));
#7133=CARTESIAN_POINT('Origin',(0.,-0.28578,0.));
#7134=CARTESIAN_POINT('',(-0.989696097314,-0.04763,-0.242834539687906));
#7135=CARTESIAN_POINT('Ctrl Pts',(-1.019052,-0.246942143572133,1.2490009027033E-16));
#7136=CARTESIAN_POINT('Ctrl Pts',(-1.019052,-0.246942143572133,-0.0206568624125605));
#7137=CARTESIAN_POINT('Ctrl Pts',(-1.01837060663223,-0.244234834628584,
-0.0430711894098822));
#7138=CARTESIAN_POINT('Ctrl Pts',(-1.0156297872271,-0.232742381310829,-0.0861971848975941));
#7139=CARTESIAN_POINT('Ctrl Pts',(-1.01358704779679,-0.223955109275652,
-0.106909345252087));
#7140=CARTESIAN_POINT('Ctrl Pts',(-1.00869718865384,-0.201072148666546,
-0.1465689792446));
#7141=CARTESIAN_POINT('Ctrl Pts',(-1.00492400591205,-0.181890537957859,
-0.169940289819232));
#7142=CARTESIAN_POINT('Ctrl Pts',(-0.998375294985966,-0.141695629206859,
-0.205111543747588));
#7143=CARTESIAN_POINT('Ctrl Pts',(-0.994830026707808,-0.11549207705665,
-0.221129100087819));
#7144=CARTESIAN_POINT('Ctrl Pts',(-0.991238884025248,-0.0742967091364495,
-0.236509675094874));
#7145=CARTESIAN_POINT('Ctrl Pts',(-0.990332542620729,-0.0609922781173484,
-0.24024064412003));
#7146=CARTESIAN_POINT('Ctrl Pts',(-0.989696097314,-0.0476300000000001,-0.242834539687907));
#7147=CARTESIAN_POINT('',(-0.871530771444223,-0.04763,-0.528110872004958));
#7148=CARTESIAN_POINT('Origin',(0.,-0.04763,0.));
#7149=CARTESIAN_POINT('',(-0.528110872004958,-0.04763,-0.871530771444223));
#7150=CARTESIAN_POINT('Ctrl Pts',(-0.871530771444223,-0.0476300000000001,
-0.528110872004958));
#7151=CARTESIAN_POINT('Ctrl Pts',(-0.87014664509073,-0.0609922781173484,
-0.530395067942936));
#7152=CARTESIAN_POINT('Ctrl Pts',(-0.868149331745851,-0.0742967091364494,
-0.533674141594226));
#7153=CARTESIAN_POINT('Ctrl Pts',(-0.85981294420286,-0.115492077056649,
-0.54708917182331));
#7154=CARTESIAN_POINT('Ctrl Pts',(-0.850993704737257,-0.141695629206859,
-0.560922177770136));
#7155=CARTESIAN_POINT('Ctrl Pts',(-0.830754510485543,-0.181890537957859,
-0.590422647829571));
#7156=CARTESIAN_POINT('Ctrl Pts',(-0.816896541396381,-0.201072148666546,
-0.609616703125488));
#7157=CARTESIAN_POINT('Ctrl Pts',(-0.792310597819928,-0.223955109275652,
-0.641117951819999));
#7158=CARTESIAN_POINT('Ctrl Pts',(-0.779109323683611,-0.232742381310829,
-0.657208095763053));
#7159=CARTESIAN_POINT('Ctrl Pts',(-0.750552691816205,-0.244234834628584,
-0.68964083160521));
#7160=CARTESIAN_POINT('Ctrl Pts',(-0.735185187071673,-0.246942143572133,
-0.705971972091755));
#7161=CARTESIAN_POINT('Ctrl Pts',(-0.705971972091754,-0.246942143572133,
-0.735185187071673));
#7162=CARTESIAN_POINT('Ctrl Pts',(-0.68964083160521,-0.244234834628584,
-0.750552691816206));
#7163=CARTESIAN_POINT('Ctrl Pts',(-0.657208095763052,-0.232742381310829,
-0.779109323683612));
#7164=CARTESIAN_POINT('Ctrl Pts',(-0.641117951819998,-0.223955109275652,
-0.792310597819928));
#7165=CARTESIAN_POINT('Ctrl Pts',(-0.609616703125488,-0.201072148666545,
-0.816896541396381));
#7166=CARTESIAN_POINT('Ctrl Pts',(-0.590422647829571,-0.181890537957859,
-0.830754510485543));
#7167=CARTESIAN_POINT('Ctrl Pts',(-0.560922177770136,-0.141695629206859,
-0.850993704737257));
#7168=CARTESIAN_POINT('Ctrl Pts',(-0.54708917182331,-0.115492077056649,
-0.85981294420286));
#7169=CARTESIAN_POINT('Ctrl Pts',(-0.533674141594226,-0.0742967091364494,
-0.868149331745852));
#7170=CARTESIAN_POINT('Ctrl Pts',(-0.530395067942936,-0.0609922781173484,
-0.870146645090731));
#7171=CARTESIAN_POINT('Ctrl Pts',(-0.528110872004958,-0.0476300000000001,
-0.871530771444223));
#7172=CARTESIAN_POINT('',(-0.242834539687906,-0.04763,-0.989696097314));
#7173=CARTESIAN_POINT('Origin',(0.,-0.04763,0.));
#7174=CARTESIAN_POINT('',(0.242834539687906,-0.04763,-0.989696097314));
#7175=CARTESIAN_POINT('Ctrl Pts',(-0.242834539687907,-0.04763,-0.989696097314));
#7176=CARTESIAN_POINT('Ctrl Pts',(-0.24024064412003,-0.0609922781173483,
-0.990332542620729));
#7177=CARTESIAN_POINT('Ctrl Pts',(-0.236509675094874,-0.0742967091364493,
-0.991238884025248));
#7178=CARTESIAN_POINT('Ctrl Pts',(-0.221129100087819,-0.115492077056649,
-0.994830026707808));
#7179=CARTESIAN_POINT('Ctrl Pts',(-0.205111543747588,-0.141695629206859,
-0.998375294985966));
#7180=CARTESIAN_POINT('Ctrl Pts',(-0.169940289819232,-0.181890537957859,
-1.00492400591205));
#7181=CARTESIAN_POINT('Ctrl Pts',(-0.1465689792446,-0.201072148666545,-1.00869718865384));
#7182=CARTESIAN_POINT('Ctrl Pts',(-0.106909345252087,-0.223955109275652,
-1.01358704779679));
#7183=CARTESIAN_POINT('Ctrl Pts',(-0.0861971848975942,-0.232742381310829,
-1.0156297872271));
#7184=CARTESIAN_POINT('Ctrl Pts',(-0.0430711894098823,-0.244234834628584,
-1.01837060663223));
#7185=CARTESIAN_POINT('Ctrl Pts',(-0.0206568624125606,-0.246942143572133,
-1.019052));
#7186=CARTESIAN_POINT('Ctrl Pts',(0.0206568624125607,-0.246942143572133,
-1.019052));
#7187=CARTESIAN_POINT('Ctrl Pts',(0.0430711894098824,-0.244234834628584,
-1.01837060663223));
#7188=CARTESIAN_POINT('Ctrl Pts',(0.0861971848975943,-0.232742381310829,
-1.0156297872271));
#7189=CARTESIAN_POINT('Ctrl Pts',(0.106909345252088,-0.223955109275652,
-1.01358704779679));
#7190=CARTESIAN_POINT('Ctrl Pts',(0.1465689792446,-0.201072148666545,-1.00869718865384));
#7191=CARTESIAN_POINT('Ctrl Pts',(0.169940289819232,-0.181890537957859,
-1.00492400591205));
#7192=CARTESIAN_POINT('Ctrl Pts',(0.205111543747588,-0.141695629206859,
-0.998375294985966));
#7193=CARTESIAN_POINT('Ctrl Pts',(0.221129100087819,-0.115492077056649,
-0.994830026707808));
#7194=CARTESIAN_POINT('Ctrl Pts',(0.236509675094874,-0.0742967091364493,
-0.991238884025248));
#7195=CARTESIAN_POINT('Ctrl Pts',(0.24024064412003,-0.0609922781173484,
-0.990332542620729));
#7196=CARTESIAN_POINT('Ctrl Pts',(0.242834539687907,-0.04763,-0.989696097314));
#7197=CARTESIAN_POINT('',(0.528110872004958,-0.04763,-0.871530771444223));
#7198=CARTESIAN_POINT('Origin',(0.,-0.04763,0.));
#7199=CARTESIAN_POINT('',(0.871530771444223,-0.04763,-0.528110872004958));
#7200=CARTESIAN_POINT('Ctrl Pts',(0.528110872004958,-0.0476300000000001,
-0.871530771444223));
#7201=CARTESIAN_POINT('Ctrl Pts',(0.530395067942936,-0.0609922781173484,
-0.870146645090731));
#7202=CARTESIAN_POINT('Ctrl Pts',(0.533674141594226,-0.0742967091364493,
-0.868149331745851));
#7203=CARTESIAN_POINT('Ctrl Pts',(0.54708917182331,-0.115492077056649,-0.85981294420286));
#7204=CARTESIAN_POINT('Ctrl Pts',(0.560922177770136,-0.141695629206859,
-0.850993704737257));
#7205=CARTESIAN_POINT('Ctrl Pts',(0.590422647829571,-0.181890537957859,
-0.830754510485543));
#7206=CARTESIAN_POINT('Ctrl Pts',(0.609616703125488,-0.201072148666545,
-0.816896541396381));
#7207=CARTESIAN_POINT('Ctrl Pts',(0.641117951819998,-0.223955109275652,
-0.792310597819928));
#7208=CARTESIAN_POINT('Ctrl Pts',(0.657208095763053,-0.232742381310829,
-0.779109323683612));
#7209=CARTESIAN_POINT('Ctrl Pts',(0.68964083160521,-0.244234834628584,-0.750552691816206));
#7210=CARTESIAN_POINT('Ctrl Pts',(0.705971972091755,-0.246942143572133,
-0.735185187071673));
#7211=CARTESIAN_POINT('Ctrl Pts',(0.735185187071673,-0.246942143572133,
-0.705971972091754));
#7212=CARTESIAN_POINT('Ctrl Pts',(0.750552691816206,-0.244234834628584,
-0.68964083160521));
#7213=CARTESIAN_POINT('Ctrl Pts',(0.779109323683612,-0.232742381310829,
-0.657208095763053));
#7214=CARTESIAN_POINT('Ctrl Pts',(0.792310597819928,-0.223955109275652,
-0.641117951819998));
#7215=CARTESIAN_POINT('Ctrl Pts',(0.816896541396381,-0.201072148666545,
-0.609616703125488));
#7216=CARTESIAN_POINT('Ctrl Pts',(0.830754510485543,-0.181890537957859,
-0.590422647829571));
#7217=CARTESIAN_POINT('Ctrl Pts',(0.850993704737257,-0.141695629206859,
-0.560922177770136));
#7218=CARTESIAN_POINT('Ctrl Pts',(0.85981294420286,-0.115492077056649,-0.54708917182331));
#7219=CARTESIAN_POINT('Ctrl Pts',(0.868149331745851,-0.0742967091364493,
-0.533674141594226));
#7220=CARTESIAN_POINT('Ctrl Pts',(0.870146645090731,-0.0609922781173484,
-0.530395067942936));
#7221=CARTESIAN_POINT('Ctrl Pts',(0.871530771444223,-0.0476300000000001,
-0.528110872004958));
#7222=CARTESIAN_POINT('',(0.989696097314,-0.04763,-0.242834539687906));
#7223=CARTESIAN_POINT('Origin',(0.,-0.04763,0.));
#7224=CARTESIAN_POINT('',(0.989696097314,-0.04763,0.242834539687906));
#7225=CARTESIAN_POINT('Ctrl Pts',(0.989696097314,-0.04763,-0.242834539687907));
#7226=CARTESIAN_POINT('Ctrl Pts',(0.990332542620729,-0.0609922781173483,
-0.24024064412003));
#7227=CARTESIAN_POINT('Ctrl Pts',(0.991238884025248,-0.0742967091364493,
-0.236509675094874));
#7228=CARTESIAN_POINT('Ctrl Pts',(0.994830026707808,-0.115492077056649,
-0.221129100087819));
#7229=CARTESIAN_POINT('Ctrl Pts',(0.998375294985966,-0.141695629206859,
-0.205111543747588));
#7230=CARTESIAN_POINT('Ctrl Pts',(1.00492400591205,-0.181890537957859,-0.169940289819232));
#7231=CARTESIAN_POINT('Ctrl Pts',(1.00869718865384,-0.201072148666545,-0.1465689792446));
#7232=CARTESIAN_POINT('Ctrl Pts',(1.01358704779679,-0.223955109275652,-0.106909345252087));
#7233=CARTESIAN_POINT('Ctrl Pts',(1.0156297872271,-0.232742381310829,-0.0861971848975942));
#7234=CARTESIAN_POINT('Ctrl Pts',(1.01837060663223,-0.244234834628584,-0.0430711894098823));
#7235=CARTESIAN_POINT('Ctrl Pts',(1.019052,-0.246942143572133,-0.0206568624125607));
#7236=CARTESIAN_POINT('Ctrl Pts',(1.019052,-0.246942143572133,0.0206568624125607));
#7237=CARTESIAN_POINT('Ctrl Pts',(1.01837060663223,-0.244234834628584,0.0430711894098823));
#7238=CARTESIAN_POINT('Ctrl Pts',(1.0156297872271,-0.232742381310829,0.0861971848975942));
#7239=CARTESIAN_POINT('Ctrl Pts',(1.01358704779679,-0.223955109275652,0.106909345252087));
#7240=CARTESIAN_POINT('Ctrl Pts',(1.00869718865384,-0.201072148666545,0.1465689792446));
#7241=CARTESIAN_POINT('Ctrl Pts',(1.00492400591205,-0.181890537957859,0.169940289819232));
#7242=CARTESIAN_POINT('Ctrl Pts',(0.998375294985966,-0.141695629206859,
0.205111543747588));
#7243=CARTESIAN_POINT('Ctrl Pts',(0.994830026707808,-0.115492077056649,
0.221129100087819));
#7244=CARTESIAN_POINT('Ctrl Pts',(0.991238884025248,-0.0742967091364492,
0.236509675094874));
#7245=CARTESIAN_POINT('Ctrl Pts',(0.990332542620729,-0.0609922781173483,
0.24024064412003));
#7246=CARTESIAN_POINT('Ctrl Pts',(0.989696097314,-0.04763,0.242834539687907));
#7247=CARTESIAN_POINT('Origin',(0.,-0.04763,0.));
#7248=CARTESIAN_POINT('Origin',(0.,-0.04763,0.));
#7249=CARTESIAN_POINT('',(0.238183666596899,-0.04763,0.951592097314));
#7250=CARTESIAN_POINT('Origin',(0.,-0.04763,0.));
#7251=CARTESIAN_POINT('Origin',(-1.94289029309402E-16,-0.04763,1.));
#7252=CARTESIAN_POINT('Origin',(-1.94289029309402E-16,0.,1.));
#7253=CARTESIAN_POINT('',(-0.2381836665969,-0.04763,0.951592097314));
#7254=CARTESIAN_POINT('Ctrl Pts',(-0.238183666596899,-0.0476299999999999,
0.951592097314));
#7255=CARTESIAN_POINT('Ctrl Pts',(-0.233157223576062,-0.0740444353928835,
0.952850216871763));
#7256=CARTESIAN_POINT('Ctrl Pts',(-0.223801617934946,-0.0999305678883309,
0.955173119738174));
#7257=CARTESIAN_POINT('Ctrl Pts',(-0.199966927975188,-0.142345102874864,
0.960411259488514));
#7258=CARTESIAN_POINT('Ctrl Pts',(-0.1868781821531,-0.159766064500479,0.963103647174702));
#7259=CARTESIAN_POINT('Ctrl Pts',(-0.15681442133453,-0.190326085855194,
0.968453058988463));
#7260=CARTESIAN_POINT('Ctrl Pts',(-0.139836317888043,-0.203463743702801,
0.971100730005489));
#7261=CARTESIAN_POINT('Ctrl Pts',(-0.104422493053067,-0.224161999508995,
0.975530745318961));
#7262=CARTESIAN_POINT('Ctrl Pts',(-0.0842175114474176,-0.232861760990032,
0.977553872336861));
#7263=CARTESIAN_POINT('Ctrl Pts',(-0.0421062857595701,-0.244251601209411,
0.980270995488453));
#7264=CARTESIAN_POINT('Ctrl Pts',(-0.0201990724523197,-0.246942143572133,
0.980948));
#7265=CARTESIAN_POINT('Ctrl Pts',(0.020199072452319,-0.246942143572133,
0.980948));
#7266=CARTESIAN_POINT('Ctrl Pts',(0.0421062857595694,-0.244251601209411,
0.980270995488454));
#7267=CARTESIAN_POINT('Ctrl Pts',(0.0842175114474169,-0.232861760990032,
0.977553872336861));
#7268=CARTESIAN_POINT('Ctrl Pts',(0.104422493053067,-0.224161999508995,
0.975530745318961));
#7269=CARTESIAN_POINT('Ctrl Pts',(0.139836317888042,-0.203463743702801,
0.971100730005489));
#7270=CARTESIAN_POINT('Ctrl Pts',(0.15681442133453,-0.190326085855194,0.968453058988463));
#7271=CARTESIAN_POINT('Ctrl Pts',(0.1868781821531,-0.15976606450048,0.963103647174702));
#7272=CARTESIAN_POINT('Ctrl Pts',(0.199966927975188,-0.142345102874864,
0.960411259488514));
#7273=CARTESIAN_POINT('Ctrl Pts',(0.223801617934945,-0.0999305678883309,
0.955173119738174));
#7274=CARTESIAN_POINT('Ctrl Pts',(0.233157223576061,-0.0740444353928835,
0.952850216871763));
#7275=CARTESIAN_POINT('Ctrl Pts',(0.238183666596899,-0.0476299999999999,
0.951592097314));
#7276=CARTESIAN_POINT('Origin',(-1.94289029309402E-16,-0.04763,1.));
#7277=CARTESIAN_POINT('Origin',(0.,-0.04763,0.));
#7278=CARTESIAN_POINT('',(-0.504455939115715,-0.04763,0.841298510752802));
#7279=CARTESIAN_POINT('Origin',(0.,-0.04763,0.));
#7280=CARTESIAN_POINT('Origin',(-0.707106781186548,-0.04763,0.707106781186547));
#7281=CARTESIAN_POINT('Origin',(-0.707106781186548,0.,0.707106781186547));
#7282=CARTESIAN_POINT('',(-0.841298510752802,-0.04763,0.504455939115715));
#7283=CARTESIAN_POINT('Ctrl Pts',(-0.841298510752802,-0.04763,0.504455939115715));
#7284=CARTESIAN_POINT('Ctrl Pts',(-0.838633903678357,-0.0740444353928835,
0.508899795931835));
#7285=CARTESIAN_POINT('Ctrl Pts',(-0.833661031856294,-0.0999305678883309,
0.517157748491652));
#7286=CARTESIAN_POINT('Ctrl Pts',(-0.820511285096538,-0.142345102874864,
0.537715343527944));
#7287=CARTESIAN_POINT('Ctrl Pts',(-0.813159949759,-0.159766064500479,0.548874290046456));
#7288=CARTESIAN_POINT('Ctrl Pts',(-0.795684265985089,-0.190326085855194,
0.573915184558107));
#7289=CARTESIAN_POINT('Ctrl Pts',(-0.78555112003688,-0.203463743702801,
0.587792702767295));
#7290=CARTESIAN_POINT('Ctrl Pts',(-0.763642258217233,-0.224161999508995,
0.615966552324775));
#7291=CARTESIAN_POINT('Ctrl Pts',(-0.750785745543687,-0.232861760990032,
0.631684198665438));
#7292=CARTESIAN_POINT('Ctrl Pts',(-0.722929908501543,-0.244251601209411,
0.663382628119203));
#7293=CARTESIAN_POINT('Ctrl Pts',(-0.707917883896095,-0.246942143572133,
0.679352081686668));
#7294=CARTESIAN_POINT('Ctrl Pts',(-0.679352081686668,-0.246942143572133,
0.707917883896095));
#7295=CARTESIAN_POINT('Ctrl Pts',(-0.663382628119203,-0.244251601209411,
0.722929908501544));
#7296=CARTESIAN_POINT('Ctrl Pts',(-0.631684198665438,-0.232861760990031,
0.750785745543687));
#7297=CARTESIAN_POINT('Ctrl Pts',(-0.615966552324775,-0.224161999508995,
0.763642258217233));
#7298=CARTESIAN_POINT('Ctrl Pts',(-0.587792702767295,-0.203463743702801,
0.78555112003688));
#7299=CARTESIAN_POINT('Ctrl Pts',(-0.573915184558107,-0.190326085855194,
0.795684265985088));
#7300=CARTESIAN_POINT('Ctrl Pts',(-0.548874290046456,-0.159766064500479,
0.813159949759));
#7301=CARTESIAN_POINT('Ctrl Pts',(-0.537715343527944,-0.142345102874864,
0.820511285096538));
#7302=CARTESIAN_POINT('Ctrl Pts',(-0.517157748491652,-0.0999305678883309,
0.833661031856294));
#7303=CARTESIAN_POINT('Ctrl Pts',(-0.508899795931835,-0.0740444353928835,
0.838633903678357));
#7304=CARTESIAN_POINT('Ctrl Pts',(-0.504455939115716,-0.04763,0.841298510752801));
#7305=CARTESIAN_POINT('Origin',(-0.707106781186548,-0.04763,0.707106781186547));
#7306=CARTESIAN_POINT('Origin',(0.,-0.04763,0.));
#7307=CARTESIAN_POINT('',(-0.951592097314,-0.04763,0.238183666596899));
#7308=CARTESIAN_POINT('Origin',(0.,-0.04763,0.));
#7309=CARTESIAN_POINT('Origin',(-1.,-0.04763,-1.11022302462516E-16));
#7310=CARTESIAN_POINT('Origin',(-1.,0.,-1.11022302462516E-16));
#7311=CARTESIAN_POINT('',(-0.951592097314,-0.04763,-0.2381836665969));
#7312=CARTESIAN_POINT('',(-0.980948,-0.246942143572133,1.08514323328844E-18));
#7313=CARTESIAN_POINT('Ctrl Pts',(-0.951592097314,-0.04763,-0.238183666596899));
#7314=CARTESIAN_POINT('Ctrl Pts',(-0.952850216871763,-0.0740444353928835,
-0.233157223576062));
#7315=CARTESIAN_POINT('Ctrl Pts',(-0.955173119738174,-0.0999305678883309,
-0.223801617934946));
#7316=CARTESIAN_POINT('Ctrl Pts',(-0.960411259488514,-0.142345102874864,
-0.199966927975188));
#7317=CARTESIAN_POINT('Ctrl Pts',(-0.963103647174702,-0.159766064500479,
-0.1868781821531));
#7318=CARTESIAN_POINT('Ctrl Pts',(-0.968453058988463,-0.190326085855194,
-0.15681442133453));
#7319=CARTESIAN_POINT('Ctrl Pts',(-0.971100730005489,-0.203463743702801,
-0.139836317888043));
#7320=CARTESIAN_POINT('Ctrl Pts',(-0.975530745318961,-0.224161999508995,
-0.104422493053067));
#7321=CARTESIAN_POINT('Ctrl Pts',(-0.977553872336861,-0.232861760990032,
-0.0842175114474175));
#7322=CARTESIAN_POINT('Ctrl Pts',(-0.980270995488453,-0.244251601209411,
-0.0421062857595699));
#7323=CARTESIAN_POINT('Ctrl Pts',(-0.980948,-0.246942143572133,-0.0201990724523195));
#7324=CARTESIAN_POINT('Ctrl Pts',(-0.980948,-0.246942143572133,-1.17961196366423E-16));
#7325=CARTESIAN_POINT('Origin',(-1.,-0.04763,-1.11022302462516E-16));
#7326=CARTESIAN_POINT('Ctrl Pts',(-0.980948,-0.246942143572133,-1.17961196366423E-16));
#7327=CARTESIAN_POINT('Ctrl Pts',(-0.980948,-0.246942143572133,0.0201990724523192));
#7328=CARTESIAN_POINT('Ctrl Pts',(-0.980270995488453,-0.244251601209411,
0.0421062857595695));
#7329=CARTESIAN_POINT('Ctrl Pts',(-0.977553872336861,-0.232861760990032,
0.0842175114474169));
#7330=CARTESIAN_POINT('Ctrl Pts',(-0.975530745318961,-0.224161999508995,
0.104422493053066));
#7331=CARTESIAN_POINT('Ctrl Pts',(-0.971100730005489,-0.203463743702801,
0.139836317888042));
#7332=CARTESIAN_POINT('Ctrl Pts',(-0.968453058988463,-0.190326085855194,
0.15681442133453));
#7333=CARTESIAN_POINT('Ctrl Pts',(-0.963103647174702,-0.15976606450048,
0.1868781821531));
#7334=CARTESIAN_POINT('Ctrl Pts',(-0.960411259488514,-0.142345102874864,
0.199966927975188));
#7335=CARTESIAN_POINT('Ctrl Pts',(-0.955173119738174,-0.099930567888331,
0.223801617934945));
#7336=CARTESIAN_POINT('Ctrl Pts',(-0.952850216871763,-0.0740444353928835,
0.233157223576061));
#7337=CARTESIAN_POINT('Ctrl Pts',(-0.951592097314,-0.04763,0.238183666596899));
#7338=CARTESIAN_POINT('Origin',(0.,-0.04763,0.));
#7339=CARTESIAN_POINT('',(-0.841298510752802,-0.04763,-0.504455939115715));
#7340=CARTESIAN_POINT('Origin',(0.,-0.04763,0.));
#7341=CARTESIAN_POINT('Origin',(-0.707106781186547,-0.04763,-0.707106781186548));
#7342=CARTESIAN_POINT('Origin',(-0.707106781186547,0.,-0.707106781186548));
#7343=CARTESIAN_POINT('',(-0.504455939115715,-0.04763,-0.841298510752802));
#7344=CARTESIAN_POINT('Ctrl Pts',(-0.504455939115715,-0.04763,-0.841298510752802));
#7345=CARTESIAN_POINT('Ctrl Pts',(-0.508899795931835,-0.0740444353928835,
-0.838633903678357));
#7346=CARTESIAN_POINT('Ctrl Pts',(-0.517157748491652,-0.0999305678883309,
-0.833661031856294));
#7347=CARTESIAN_POINT('Ctrl Pts',(-0.537715343527944,-0.142345102874864,
-0.820511285096538));
#7348=CARTESIAN_POINT('Ctrl Pts',(-0.548874290046456,-0.159766064500479,
-0.813159949759));
#7349=CARTESIAN_POINT('Ctrl Pts',(-0.573915184558107,-0.190326085855194,
-0.795684265985089));
#7350=CARTESIAN_POINT('Ctrl Pts',(-0.587792702767295,-0.203463743702801,
-0.78555112003688));
#7351=CARTESIAN_POINT('Ctrl Pts',(-0.615966552324775,-0.224161999508995,
-0.763642258217233));
#7352=CARTESIAN_POINT('Ctrl Pts',(-0.631684198665438,-0.232861760990032,
-0.750785745543687));
#7353=CARTESIAN_POINT('Ctrl Pts',(-0.663382628119203,-0.244251601209411,
-0.722929908501543));
#7354=CARTESIAN_POINT('Ctrl Pts',(-0.679352081686668,-0.246942143572133,
-0.707917883896095));
#7355=CARTESIAN_POINT('Ctrl Pts',(-0.707917883896095,-0.246942143572133,
-0.679352081686668));
#7356=CARTESIAN_POINT('Ctrl Pts',(-0.722929908501543,-0.244251601209411,
-0.663382628119203));
#7357=CARTESIAN_POINT('Ctrl Pts',(-0.750785745543687,-0.232861760990032,
-0.631684198665439));
#7358=CARTESIAN_POINT('Ctrl Pts',(-0.763642258217232,-0.224161999508995,
-0.615966552324775));
#7359=CARTESIAN_POINT('Ctrl Pts',(-0.78555112003688,-0.203463743702801,
-0.587792702767295));
#7360=CARTESIAN_POINT('Ctrl Pts',(-0.795684265985088,-0.190326085855194,
-0.573915184558107));
#7361=CARTESIAN_POINT('Ctrl Pts',(-0.813159949759,-0.15976606450048,-0.548874290046456));
#7362=CARTESIAN_POINT('Ctrl Pts',(-0.820511285096538,-0.142345102874864,
-0.537715343527944));
#7363=CARTESIAN_POINT('Ctrl Pts',(-0.833661031856294,-0.0999305678883311,
-0.517157748491652));
#7364=CARTESIAN_POINT('Ctrl Pts',(-0.838633903678357,-0.0740444353928836,
-0.508899795931835));
#7365=CARTESIAN_POINT('Ctrl Pts',(-0.841298510752801,-0.04763,-0.504455939115715));
#7366=CARTESIAN_POINT('Origin',(-0.707106781186547,-0.04763,-0.707106781186548));
#7367=CARTESIAN_POINT('Origin',(0.,-0.04763,0.));
#7368=CARTESIAN_POINT('',(-0.238183666596899,-0.04763,-0.951592097314));
#7369=CARTESIAN_POINT('Origin',(0.,-0.04763,0.));
#7370=CARTESIAN_POINT('Origin',(5.55111512312578E-17,-0.04763,-1.));
#7371=CARTESIAN_POINT('Origin',(5.55111512312578E-17,0.,-1.));
#7372=CARTESIAN_POINT('',(0.238183666596899,-0.04763,-0.951592097314));
#7373=CARTESIAN_POINT('Ctrl Pts',(0.238183666596899,-0.04763,-0.951592097314));
#7374=CARTESIAN_POINT('Ctrl Pts',(0.233157223576062,-0.0740444353928835,
-0.952850216871763));
#7375=CARTESIAN_POINT('Ctrl Pts',(0.223801617934946,-0.099930567888331,
-0.955173119738174));
#7376=CARTESIAN_POINT('Ctrl Pts',(0.199966927975188,-0.142345102874864,
-0.960411259488514));
#7377=CARTESIAN_POINT('Ctrl Pts',(0.1868781821531,-0.15976606450048,-0.963103647174702));
#7378=CARTESIAN_POINT('Ctrl Pts',(0.15681442133453,-0.190326085855194,-0.968453058988463));
#7379=CARTESIAN_POINT('Ctrl Pts',(0.139836317888042,-0.203463743702801,
-0.971100730005489));
#7380=CARTESIAN_POINT('Ctrl Pts',(0.104422493053067,-0.224161999508995,
-0.975530745318961));
#7381=CARTESIAN_POINT('Ctrl Pts',(0.0842175114474173,-0.232861760990032,
-0.977553872336861));
#7382=CARTESIAN_POINT('Ctrl Pts',(0.0421062857595698,-0.244251601209411,
-0.980270995488453));
#7383=CARTESIAN_POINT('Ctrl Pts',(0.0201990724523194,-0.246942143572133,
-0.980948));
#7384=CARTESIAN_POINT('Ctrl Pts',(-0.0201990724523193,-0.246942143572133,
-0.980948));
#7385=CARTESIAN_POINT('Ctrl Pts',(-0.0421062857595697,-0.244251601209411,
-0.980270995488453));
#7386=CARTESIAN_POINT('Ctrl Pts',(-0.0842175114474171,-0.232861760990032,
-0.977553872336861));
#7387=CARTESIAN_POINT('Ctrl Pts',(-0.104422493053067,-0.224161999508995,
-0.975530745318961));
#7388=CARTESIAN_POINT('Ctrl Pts',(-0.139836317888042,-0.203463743702801,
-0.971100730005489));
#7389=CARTESIAN_POINT('Ctrl Pts',(-0.15681442133453,-0.190326085855194,
-0.968453058988463));
#7390=CARTESIAN_POINT('Ctrl Pts',(-0.1868781821531,-0.15976606450048,-0.963103647174702));
#7391=CARTESIAN_POINT('Ctrl Pts',(-0.199966927975188,-0.142345102874864,
-0.960411259488514));
#7392=CARTESIAN_POINT('Ctrl Pts',(-0.223801617934945,-0.099930567888331,
-0.955173119738174));
#7393=CARTESIAN_POINT('Ctrl Pts',(-0.233157223576062,-0.0740444353928835,
-0.952850216871763));
#7394=CARTESIAN_POINT('Ctrl Pts',(-0.238183666596899,-0.0476299999999999,
-0.951592097314));
#7395=CARTESIAN_POINT('Origin',(5.55111512312578E-17,-0.04763,-1.));
#7396=CARTESIAN_POINT('Origin',(0.,-0.04763,0.));
#7397=CARTESIAN_POINT('',(0.504455939115715,-0.04763,-0.841298510752802));
#7398=CARTESIAN_POINT('Origin',(0.,-0.04763,0.));
#7399=CARTESIAN_POINT('Origin',(0.707106781186548,-0.04763,-0.707106781186547));
#7400=CARTESIAN_POINT('Origin',(0.707106781186548,0.,-0.707106781186547));
#7401=CARTESIAN_POINT('',(0.841298510752802,-0.04763,-0.504455939115715));
#7402=CARTESIAN_POINT('Ctrl Pts',(0.841298510752802,-0.04763,-0.504455939115715));
#7403=CARTESIAN_POINT('Ctrl Pts',(0.838633903678357,-0.0740444353928835,
-0.508899795931835));
#7404=CARTESIAN_POINT('Ctrl Pts',(0.833661031856294,-0.0999305678883309,
-0.517157748491652));
#7405=CARTESIAN_POINT('Ctrl Pts',(0.820511285096538,-0.142345102874864,
-0.537715343527944));
#7406=CARTESIAN_POINT('Ctrl Pts',(0.813159949759,-0.159766064500479,-0.548874290046456));
#7407=CARTESIAN_POINT('Ctrl Pts',(0.795684265985088,-0.190326085855194,
-0.573915184558107));
#7408=CARTESIAN_POINT('Ctrl Pts',(0.78555112003688,-0.203463743702801,-0.587792702767295));
#7409=CARTESIAN_POINT('Ctrl Pts',(0.763642258217233,-0.224161999508995,
-0.615966552324775));
#7410=CARTESIAN_POINT('Ctrl Pts',(0.750785745543687,-0.232861760990032,
-0.631684198665438));
#7411=CARTESIAN_POINT('Ctrl Pts',(0.722929908501543,-0.244251601209411,
-0.663382628119203));
#7412=CARTESIAN_POINT('Ctrl Pts',(0.707917883896095,-0.246942143572133,
-0.679352081686668));
#7413=CARTESIAN_POINT('Ctrl Pts',(0.679352081686668,-0.246942143572133,
-0.707917883896095));
#7414=CARTESIAN_POINT('Ctrl Pts',(0.663382628119203,-0.244251601209411,
-0.722929908501543));
#7415=CARTESIAN_POINT('Ctrl Pts',(0.631684198665438,-0.232861760990032,
-0.750785745543687));
#7416=CARTESIAN_POINT('Ctrl Pts',(0.615966552324775,-0.224161999508995,
-0.763642258217232));
#7417=CARTESIAN_POINT('Ctrl Pts',(0.587792702767295,-0.203463743702801,
-0.78555112003688));
#7418=CARTESIAN_POINT('Ctrl Pts',(0.573915184558107,-0.190326085855194,
-0.795684265985088));
#7419=CARTESIAN_POINT('Ctrl Pts',(0.548874290046456,-0.159766064500479,
-0.813159949759));
#7420=CARTESIAN_POINT('Ctrl Pts',(0.537715343527944,-0.142345102874864,
-0.820511285096538));
#7421=CARTESIAN_POINT('Ctrl Pts',(0.517157748491652,-0.099930567888331,
-0.833661031856294));
#7422=CARTESIAN_POINT('Ctrl Pts',(0.508899795931835,-0.0740444353928835,
-0.838633903678357));
#7423=CARTESIAN_POINT('Ctrl Pts',(0.504455939115715,-0.04763,-0.841298510752801));
#7424=CARTESIAN_POINT('Origin',(0.707106781186548,-0.04763,-0.707106781186547));
#7425=CARTESIAN_POINT('Origin',(0.,-0.166705,0.));
#7426=CARTESIAN_POINT('',(-0.980948,-0.28578,1.20131482833E-16));
#7427=CARTESIAN_POINT('Origin',(0.,-0.28578,0.));
#7428=CARTESIAN_POINT('',(-0.980948,-0.166705,1.20131482833E-16));
#7429=CARTESIAN_POINT('',(0.951592097314,-0.04763,0.238183666596899));
#7430=CARTESIAN_POINT('Origin',(0.,-0.04763,0.));
#7431=CARTESIAN_POINT('',(0.951592097314,-0.04763,-0.238183666596899));
#7432=CARTESIAN_POINT('Ctrl Pts',(0.951592097314,-0.04763,0.238183666596899));
#7433=CARTESIAN_POINT('Ctrl Pts',(0.952850216871763,-0.0740444353928835,
0.233157223576062));
#7434=CARTESIAN_POINT('Ctrl Pts',(0.955173119738174,-0.099930567888331,
0.223801617934945));
#7435=CARTESIAN_POINT('Ctrl Pts',(0.960411259488514,-0.142345102874864,
0.199966927975188));
#7436=CARTESIAN_POINT('Ctrl Pts',(0.963103647174702,-0.15976606450048,0.1868781821531));
#7437=CARTESIAN_POINT('Ctrl Pts',(0.968453058988463,-0.190326085855194,
0.15681442133453));
#7438=CARTESIAN_POINT('Ctrl Pts',(0.971100730005489,-0.203463743702801,
0.139836317888042));
#7439=CARTESIAN_POINT('Ctrl Pts',(0.975530745318961,-0.224161999508995,
0.104422493053067));
#7440=CARTESIAN_POINT('Ctrl Pts',(0.977553872336861,-0.232861760990032,
0.0842175114474172));
#7441=CARTESIAN_POINT('Ctrl Pts',(0.980270995488453,-0.244251601209411,
0.0421062857595697));
#7442=CARTESIAN_POINT('Ctrl Pts',(0.980948,-0.246942143572133,0.0201990724523194));
#7443=CARTESIAN_POINT('Ctrl Pts',(0.980948,-0.246942143572133,-0.0201990724523194));
#7444=CARTESIAN_POINT('Ctrl Pts',(0.980270995488453,-0.244251601209411,
-0.0421062857595697));
#7445=CARTESIAN_POINT('Ctrl Pts',(0.977553872336861,-0.232861760990032,
-0.0842175114474172));
#7446=CARTESIAN_POINT('Ctrl Pts',(0.975530745318961,-0.224161999508995,
-0.104422493053067));
#7447=CARTESIAN_POINT('Ctrl Pts',(0.971100730005489,-0.203463743702801,
-0.139836317888042));
#7448=CARTESIAN_POINT('Ctrl Pts',(0.968453058988463,-0.190326085855194,
-0.15681442133453));
#7449=CARTESIAN_POINT('Ctrl Pts',(0.963103647174702,-0.15976606450048,-0.1868781821531));
#7450=CARTESIAN_POINT('Ctrl Pts',(0.960411259488514,-0.142345102874864,
-0.199966927975188));
#7451=CARTESIAN_POINT('Ctrl Pts',(0.955173119738174,-0.099930567888331,
-0.223801617934945));
#7452=CARTESIAN_POINT('Ctrl Pts',(0.952850216871763,-0.0740444353928835,
-0.233157223576062));
#7453=CARTESIAN_POINT('Ctrl Pts',(0.951592097314,-0.0476299999999999,-0.238183666596899));
#7454=CARTESIAN_POINT('Origin',(0.,-0.04763,0.));
#7455=CARTESIAN_POINT('Origin',(0.,-0.04763,0.));
#7456=CARTESIAN_POINT('Origin',(1.,-0.04763,0.));
#7457=CARTESIAN_POINT('Origin',(1.,0.,0.));
#7458=CARTESIAN_POINT('Origin',(1.,-0.04763,0.));
#7459=CARTESIAN_POINT('Origin',(0.,-0.28578,0.));
#7460=CARTESIAN_POINT('Origin',(0.,-0.04763,0.));
#7461=CARTESIAN_POINT('',(0.,0.,0.));
#7462=CARTESIAN_POINT('Origin',(1.013815,0.445,0.));
#7463=CARTESIAN_POINT('',(-1.013815,0.445,-1.24156529467757E-16));
#7464=CARTESIAN_POINT('Origin',(0.,0.445,0.));
#7465=CARTESIAN_POINT('',(-0.991185,0.445,-1.21385153761287E-16));
#7466=CARTESIAN_POINT('Origin',(0.,0.445,0.));
#7467=CARTESIAN_POINT('Origin',(0.,0.4075,0.));
#7468=CARTESIAN_POINT('',(-1.013815,0.37,-1.24156529467757E-16));
#7469=CARTESIAN_POINT('Origin',(0.,0.37,0.));
#7470=CARTESIAN_POINT('',(-1.013815,0.4075,-1.24156529467757E-16));
#7471=CARTESIAN_POINT('Origin',(0.991185,0.37,0.));
#7472=CARTESIAN_POINT('',(-0.991185,0.37,-1.21385153761287E-16));
#7473=CARTESIAN_POINT('Origin',(0.,0.37,0.));
#7474=CARTESIAN_POINT('Origin',(0.,0.4075,0.));
#7475=CARTESIAN_POINT('',(-0.991185,0.4075,-1.21385153761287E-16));
#7476=CARTESIAN_POINT('Origin',(1.013815,-0.37,0.));
#7477=CARTESIAN_POINT('',(-1.013815,-0.37,-1.24156529467757E-16));
#7478=CARTESIAN_POINT('Origin',(0.,-0.37,0.));
#7479=CARTESIAN_POINT('',(-0.991185,-0.37,-1.21385153761287E-16));
#7480=CARTESIAN_POINT('Origin',(0.,-0.37,0.));
#7481=CARTESIAN_POINT('Origin',(0.,-0.4075,0.));
#7482=CARTESIAN_POINT('',(-1.013815,-0.445,-1.24156529467757E-16));
#7483=CARTESIAN_POINT('Origin',(0.,-0.445,0.));
#7484=CARTESIAN_POINT('',(-1.013815,-0.4075,-1.24156529467757E-16));
#7485=CARTESIAN_POINT('Origin',(0.991185,-0.445,0.));
#7486=CARTESIAN_POINT('',(-0.991185,-0.445,-1.21385153761287E-16));
#7487=CARTESIAN_POINT('Origin',(0.,-0.445,0.));
#7488=CARTESIAN_POINT('Origin',(0.,-0.4075,0.));
#7489=CARTESIAN_POINT('',(-0.991185,-0.4075,-1.21385153761287E-16));
#7490=CARTESIAN_POINT('',(0.,0.,0.));
#7491=CARTESIAN_POINT('',(0.,0.,0.));
#7492=CARTESIAN_POINT('',(0.,0.,0.));
#7493=CARTESIAN_POINT('',(0.,0.,0.));
#7494=CARTESIAN_POINT('',(0.,0.,0.));
#7495=CARTESIAN_POINT('',(0.,0.,0.));
#7496=CARTESIAN_POINT('Origin',(0.,-2.8,4.5));
#7497=CARTESIAN_POINT('',(-0.225,-2.5,4.5));
#7498=CARTESIAN_POINT('Origin',(0.,-2.5,4.5));
#7499=CARTESIAN_POINT('',(-0.225,-2.8,4.5));
#7500=CARTESIAN_POINT('',(-0.225,-2.8,4.5));
#7501=CARTESIAN_POINT('Origin',(0.,-2.8,4.5));
#7502=CARTESIAN_POINT('Origin',(0.,-2.8,4.5));
#7503=CARTESIAN_POINT('',(-1.1,-2.5,4.5));
#7504=CARTESIAN_POINT('Origin',(0.,-2.5,4.5));
#7505=CARTESIAN_POINT('',(-1.1,-2.8,4.5));
#7506=CARTESIAN_POINT('',(-1.1,-2.8,4.5));
#7507=CARTESIAN_POINT('Origin',(0.,-2.8,4.5));
#7508=CARTESIAN_POINT('Origin',(0.,-2.5,4.5));
#7509=CARTESIAN_POINT('Origin',(0.,-2.8,4.5));
#7510=CARTESIAN_POINT('',(0.,0.,0.));
#7511=CARTESIAN_POINT('Origin',(0.,-1.6,4.5));
#7512=CARTESIAN_POINT('',(-0.505,0.,4.5));
#7513=CARTESIAN_POINT('Origin',(0.,0.,4.5));
#7514=CARTESIAN_POINT('',(-0.505,-1.6,4.5));
#7515=CARTESIAN_POINT('',(-0.505,-1.6,4.5));
#7516=CARTESIAN_POINT('Origin',(0.,-1.6,4.5));
#7517=CARTESIAN_POINT('Origin',(0.,-1.6,4.5));
#7518=CARTESIAN_POINT('',(-0.8,0.,4.5));
#7519=CARTESIAN_POINT('Origin',(0.,0.,4.5));
#7520=CARTESIAN_POINT('',(-0.8,-1.6,4.5));
#7521=CARTESIAN_POINT('',(-0.8,-1.6,4.5));
#7522=CARTESIAN_POINT('Origin',(0.,-1.6,4.5));
#7523=CARTESIAN_POINT('Origin',(0.,0.,4.5));
#7524=CARTESIAN_POINT('Origin',(0.,-1.6,4.5));
#7525=CARTESIAN_POINT('',(0.,0.,0.));
#7526=CARTESIAN_POINT('Origin',(0.,-2.5,4.5));
#7527=CARTESIAN_POINT('',(-0.605,-2.4,4.5));
#7528=CARTESIAN_POINT('Origin',(0.,-2.4,4.5));
#7529=CARTESIAN_POINT('',(-0.605,-2.5,4.5));
#7530=CARTESIAN_POINT('',(-0.605,-2.5,4.5));
#7531=CARTESIAN_POINT('Origin',(0.,-2.5,4.5));
#7532=CARTESIAN_POINT('Origin',(0.,-2.5,4.5));
#7533=CARTESIAN_POINT('',(-1.,-2.4,4.5));
#7534=CARTESIAN_POINT('Origin',(0.,-2.4,4.5));
#7535=CARTESIAN_POINT('',(-1.,-2.5,4.5));
#7536=CARTESIAN_POINT('',(-1.,-2.5,4.5));
#7537=CARTESIAN_POINT('Origin',(0.,-2.5,4.5));
#7538=CARTESIAN_POINT('Origin',(0.,-2.4,4.5));
#7539=CARTESIAN_POINT('Origin',(0.,-2.5,4.5));
#7540=CARTESIAN_POINT('',(0.,0.,0.));
#7541=CARTESIAN_POINT('',(0.,0.,0.));
#7542=CARTESIAN_POINT('Origin',(0.,0.,4.5));
#7543=CARTESIAN_POINT('',(-2.2,30.,4.5));
#7544=CARTESIAN_POINT('Origin',(0.,30.,4.5));
#7545=CARTESIAN_POINT('',(-2.2,0.,4.5));
#7546=CARTESIAN_POINT('',(-2.2,0.,4.5));
#7547=CARTESIAN_POINT('Origin',(0.,0.,4.5));
#7548=CARTESIAN_POINT('Origin',(0.,0.,4.5));
#7549=CARTESIAN_POINT('',(-2.5,30.,4.5));
#7550=CARTESIAN_POINT('Origin',(0.,30.,4.5));
#7551=CARTESIAN_POINT('',(-2.5,0.,4.5));
#7552=CARTESIAN_POINT('',(-2.5,0.,4.5));
#7553=CARTESIAN_POINT('Origin',(0.,0.,4.5));
#7554=CARTESIAN_POINT('Origin',(0.,30.,4.5));
#7555=CARTESIAN_POINT('Origin',(0.,0.,4.5));
#7556=CARTESIAN_POINT('',(0.,0.,0.));
#7557=CARTESIAN_POINT('Origin',(-1.9,-0.1,4.5));
#7558=CARTESIAN_POINT('',(-2.065,0.,4.5));
#7559=CARTESIAN_POINT('Origin',(-1.9,0.,4.5));
#7560=CARTESIAN_POINT('',(-2.065,1.2,4.5));
#7561=CARTESIAN_POINT('',(-2.065,-0.1,4.5));
#7562=CARTESIAN_POINT('Origin',(-1.9,1.2,4.5));
#7563=CARTESIAN_POINT('Origin',(1.16341445918999E-16,-0.1,6.4));
#7564=CARTESIAN_POINT('',(-0.165,0.,6.4));
#7565=CARTESIAN_POINT('Origin',(1.16341445918999E-16,0.,6.4));
#7566=CARTESIAN_POINT('',(-0.165,1.2,6.4));
#7567=CARTESIAN_POINT('',(-0.165,-0.1,6.4));
#7568=CARTESIAN_POINT('Origin',(1.16341445918999E-16,1.2,6.4));
#7569=CARTESIAN_POINT('Origin',(1.9,-0.1,4.5));
#7570=CARTESIAN_POINT('',(1.735,0.,4.5));
#7571=CARTESIAN_POINT('Origin',(1.9,0.,4.5));
#7572=CARTESIAN_POINT('',(1.735,1.2,4.5));
#7573=CARTESIAN_POINT('',(1.735,-0.1,4.5));
#7574=CARTESIAN_POINT('Origin',(1.9,1.2,4.5));
#7575=CARTESIAN_POINT('Origin',(-3.49024337756996E-16,-0.1,2.6));
#7576=CARTESIAN_POINT('',(-0.165,0.,2.6));
#7577=CARTESIAN_POINT('Origin',(-3.49024337756996E-16,0.,2.6));
#7578=CARTESIAN_POINT('',(-0.165,1.2,2.6));
#7579=CARTESIAN_POINT('',(-0.165,-0.1,2.6));
#7580=CARTESIAN_POINT('Origin',(-3.49024337756996E-16,1.2,2.6));
#7581=CARTESIAN_POINT('Origin',(0.,0.9,4.5));
#7582=CARTESIAN_POINT('',(-1.2,1.2,4.5));
#7583=CARTESIAN_POINT('Origin',(0.,1.2,4.5));
#7584=CARTESIAN_POINT('',(-1.2,0.9,4.5));
#7585=CARTESIAN_POINT('',(-1.2,0.9,4.5));
#7586=CARTESIAN_POINT('Origin',(0.,0.9,4.5));
#7587=CARTESIAN_POINT('Origin',(0.,0.9,4.5));
#7588=CARTESIAN_POINT('',(-1.5,0.9,4.5));
#7589=CARTESIAN_POINT('Origin',(0.,0.9,4.5));
#7590=CARTESIAN_POINT('Origin',(0.,0.,4.5));
#7591=CARTESIAN_POINT('',(-1.5,0.,4.5));
#7592=CARTESIAN_POINT('',(-1.5,0.,4.5));
#7593=CARTESIAN_POINT('Origin',(0.,0.,4.5));
#7594=CARTESIAN_POINT('Origin',(0.,0.,4.5));
#7595=CARTESIAN_POINT('',(-2.2,1.2,4.5));
#7596=CARTESIAN_POINT('Origin',(0.,1.2,4.5));
#7597=CARTESIAN_POINT('',(-2.2,0.,4.5));
#7598=CARTESIAN_POINT('',(-2.2,0.,4.5));
#7599=CARTESIAN_POINT('Origin',(0.,0.,4.5));
#7600=CARTESIAN_POINT('Origin',(0.,1.2,4.5));
#7601=CARTESIAN_POINT('Origin',(0.,0.,4.5));
#7602=CARTESIAN_POINT('',(0.,0.,0.));
#7603=CARTESIAN_POINT('Origin',(-1.9,-0.4,4.5));
#7604=CARTESIAN_POINT('',(-2.125,-0.3,4.5));
#7605=CARTESIAN_POINT('Origin',(-1.9,-0.3,4.5));
#7606=CARTESIAN_POINT('',(-2.125,0.,4.5));
#7607=CARTESIAN_POINT('',(-2.125,-0.4,4.5));
#7608=CARTESIAN_POINT('Origin',(-1.9,0.,4.5));
#7609=CARTESIAN_POINT('Origin',(1.16341445918999E-16,-0.4,6.4));
#7610=CARTESIAN_POINT('',(-0.225,-0.3,6.4));
#7611=CARTESIAN_POINT('Origin',(1.16341445918999E-16,-0.3,6.4));
#7612=CARTESIAN_POINT('',(-0.225,0.,6.4));
#7613=CARTESIAN_POINT('',(-0.225,-0.4,6.4));
#7614=CARTESIAN_POINT('Origin',(1.16341445918999E-16,0.,6.4));
#7615=CARTESIAN_POINT('Origin',(1.9,-0.4,4.5));
#7616=CARTESIAN_POINT('',(1.675,-0.3,4.5));
#7617=CARTESIAN_POINT('Origin',(1.9,-0.3,4.5));
#7618=CARTESIAN_POINT('',(1.675,0.,4.5));
#7619=CARTESIAN_POINT('',(1.675,-0.4,4.5));
#7620=CARTESIAN_POINT('Origin',(1.9,0.,4.5));
#7621=CARTESIAN_POINT('Origin',(-3.49024337756996E-16,-0.4,2.6));
#7622=CARTESIAN_POINT('',(-0.225,-0.3,2.6));
#7623=CARTESIAN_POINT('Origin',(-3.49024337756996E-16,-0.3,2.6));
#7624=CARTESIAN_POINT('',(-0.225,0.,2.6));
#7625=CARTESIAN_POINT('',(-0.225,-0.4,2.6));
#7626=CARTESIAN_POINT('Origin',(-3.49024337756996E-16,0.,2.6));
#7627=CARTESIAN_POINT('Origin',(0.,-0.3,4.5));
#7628=CARTESIAN_POINT('',(-1.2,0.,4.5));
#7629=CARTESIAN_POINT('Origin',(0.,0.,4.5));
#7630=CARTESIAN_POINT('',(-1.2,-0.3,4.5));
#7631=CARTESIAN_POINT('',(-1.2,-0.3,4.5));
#7632=CARTESIAN_POINT('Origin',(0.,-0.3,4.5));
#7633=CARTESIAN_POINT('Origin',(0.,-0.3,4.5));
#7634=CARTESIAN_POINT('',(-2.5,0.,4.5));
#7635=CARTESIAN_POINT('Origin',(0.,0.,4.5));
#7636=CARTESIAN_POINT('',(-2.5,-0.3,4.5));
#7637=CARTESIAN_POINT('',(-2.5,-0.3,4.5));
#7638=CARTESIAN_POINT('Origin',(0.,-0.3,4.5));
#7639=CARTESIAN_POINT('Origin',(0.,0.,4.5));
#7640=CARTESIAN_POINT('Origin',(0.,-0.3,4.5));
#7641=CARTESIAN_POINT('',(0.,0.,0.));
#7642=CARTESIAN_POINT('Origin',(0.3,0.4,0.));
#7643=CARTESIAN_POINT('',(-0.3,0.4,-3.67394039744206E-17));
#7644=CARTESIAN_POINT('Origin',(0.,0.4,0.));
#7645=CARTESIAN_POINT('Origin',(0.,0.375,0.));
#7646=CARTESIAN_POINT('',(-0.35,0.35,-4.28626379701573E-17));
#7647=CARTESIAN_POINT('Origin',(0.,0.35,0.));
#7648=CARTESIAN_POINT('',(-0.325,0.375,-3.9801020972289E-17));
#7649=CARTESIAN_POINT('Origin',(0.,0.19,0.));
#7650=CARTESIAN_POINT('',(-0.35,0.03,-4.28626379701574E-17));
#7651=CARTESIAN_POINT('Origin',(0.,0.03,0.));
#7652=CARTESIAN_POINT('',(-0.35,0.19,-4.28626379701574E-17));
#7653=CARTESIAN_POINT('Origin',(0.,0.0149999999999999,0.));
#7654=CARTESIAN_POINT('',(-0.32,-3.29597460435593E-17,-3.91886975727153E-17));
#7655=CARTESIAN_POINT('Origin',(0.,0.,0.));
#7656=CARTESIAN_POINT('',(-0.335,0.0149999999999999,-4.10256677714363E-17));
#7657=CARTESIAN_POINT('Origin',(0.22,0.,0.));
#7658=CARTESIAN_POINT('',(-0.22,-6.93889390390723E-18,-2.69422295812418E-17));
#7659=CARTESIAN_POINT('Origin',(0.,0.,0.));
#7660=CARTESIAN_POINT('Origin',(0.,-0.02,0.));
#7661=CARTESIAN_POINT('',(-0.1954,-0.0492,2.39295984553393E-17));
#7662=CARTESIAN_POINT('Origin',(0.,-0.0492,0.));
#7663=CARTESIAN_POINT('',(-0.21,-0.02,-2.57175827820944E-17));
#7664=CARTESIAN_POINT('Origin',(0.,-0.8,0.));
#7665=CARTESIAN_POINT('',(-0.1954,-1.5646,2.39295984553393E-17));
#7666=CARTESIAN_POINT('Origin',(0.,-1.5646,0.));
#7667=CARTESIAN_POINT('',(-0.1954,-0.8,-2.39295984553393E-17));
#7668=CARTESIAN_POINT('Origin',(0.,-1.58,0.));
#7669=CARTESIAN_POINT('',(-0.16,-1.6,-1.95943487863577E-17));
#7670=CARTESIAN_POINT('Origin',(0.,-1.6,0.));
#7671=CARTESIAN_POINT('',(-0.18,-1.58,-2.20436423846524E-17));
#7672=CARTESIAN_POINT('Origin',(0.,-1.6,0.));
#7673=CARTESIAN_POINT('Origin',(0.0866025403784439,-0.4,-0.15));
#7674=CARTESIAN_POINT('',(0.173205080756888,-0.4,0.));
#7675=CARTESIAN_POINT('',(0.0866025403784439,-0.4,-0.15));
#7676=CARTESIAN_POINT('',(0.173205080756888,-0.4,0.));
#7677=CARTESIAN_POINT('',(0.0866025403784439,-0.64,-0.15));
#7678=CARTESIAN_POINT('',(0.0866025403784439,-0.4,-0.15));
#7679=CARTESIAN_POINT('',(0.173205080756888,-0.64,0.));
#7680=CARTESIAN_POINT('',(0.173205080756888,-0.64,0.));
#7681=CARTESIAN_POINT('',(0.173205080756888,-0.4,0.));
#7682=CARTESIAN_POINT('Origin',(-0.0866025403784438,-0.4,-0.15));
#7683=CARTESIAN_POINT('',(-0.0866025403784438,-0.4,-0.15));
#7684=CARTESIAN_POINT('',(0.0866025403784439,-0.4,-0.15));
#7685=CARTESIAN_POINT('',(-0.0866025403784438,-0.64,-0.15));
#7686=CARTESIAN_POINT('',(-0.0866025403784438,-0.4,-0.15));
#7687=CARTESIAN_POINT('',(0.0866025403784439,-0.64,-0.15));
#7688=CARTESIAN_POINT('Origin',(-0.173205080756888,-0.4,-2.77555756156289E-17));
#7689=CARTESIAN_POINT('',(-0.173205080756888,-0.4,-2.12115047744981E-17));
#7690=CARTESIAN_POINT('',(-0.0866025403784438,-0.4,-0.15));
#7691=CARTESIAN_POINT('',(-0.173205080756888,-0.64,-2.77555756156289E-17));
#7692=CARTESIAN_POINT('',(-0.173205080756888,-0.4,-2.12115047744981E-17));
#7693=CARTESIAN_POINT('',(-0.0866025403784438,-0.64,-0.15));
#7694=CARTESIAN_POINT('Origin',(-0.0866025403784439,-0.4,0.15));
#7695=CARTESIAN_POINT('',(-0.0866025403784439,-0.4,0.15));
#7696=CARTESIAN_POINT('',(-0.173205080756888,-0.4,-2.12115047744981E-17));
#7697=CARTESIAN_POINT('',(-0.0866025403784439,-0.64,0.15));
#7698=CARTESIAN_POINT('',(-0.0866025403784439,-0.4,0.15));
#7699=CARTESIAN_POINT('',(-0.173205080756888,-0.64,-2.12115047744981E-17));
#7700=CARTESIAN_POINT('Origin',(0.0866025403784439,-0.4,0.15));
#7701=CARTESIAN_POINT('',(0.0866025403784439,-0.4,0.15));
#7702=CARTESIAN_POINT('',(-0.0866025403784439,-0.4,0.15));
#7703=CARTESIAN_POINT('',(0.0866025403784439,-0.64,0.15));
#7704=CARTESIAN_POINT('',(0.0866025403784439,-0.4,0.15));
#7705=CARTESIAN_POINT('',(-0.0866025403784439,-0.64,0.15));
#7706=CARTESIAN_POINT('Origin',(0.173205080756888,-0.4,0.));
#7707=CARTESIAN_POINT('',(0.0866025403784439,-0.4,0.15));
#7708=CARTESIAN_POINT('',(0.0866025403784439,-0.64,0.15));
#7709=CARTESIAN_POINT('Origin',(0.,-0.4,-2.77555756156289E-17));
#7710=CARTESIAN_POINT('Origin',(0.,-0.64,-2.77555756156289E-17));
#7711=CARTESIAN_POINT('',(0.,-0.45,-4.5));
#7712=CARTESIAN_POINT('',(-3.,-0.45,-4.5));
#7713=CARTESIAN_POINT('',(-1.4,-2.45,-3.08));
#7714=CARTESIAN_POINT('',(1.4,-2.45,-3.08));
#7715=CARTESIAN_POINT('',(-1.4,-2.45,-1.6));
#7716=CARTESIAN_POINT('',(-3.,-0.45,-4.5));
#7717=CARTESIAN_POINT('',(1.4,-2.45,-1.6));
#7718=CARTESIAN_POINT('',(0.,29.1,0.));
#7719=CARTESIAN_POINT('',(0.,32.35,0.));
#7720=CARTESIAN_POINT('',(0.,34.45,-4.5));
#7721=CARTESIAN_POINT('',(1.4,31.55,-1.6));
#7722=CARTESIAN_POINT('',(1.4,31.55,-3.08));
#7723=CARTESIAN_POINT('',(-1.4,31.55,-1.6));
#7724=CARTESIAN_POINT('',(-1.4,31.55,-3.08));
#7725=CARTESIAN_POINT('',(0.,31.15,-4.5));
#7726=CARTESIAN_POINT('',(0.,34.85,-4.5));
#7727=CARTESIAN_POINT('',(0.,0.,0.));
#7728=CARTESIAN_POINT('',(0.,-0.45,-4.5));
#7729=CARTESIAN_POINT('',(0.,-0.45,-4.5));
#7730=CARTESIAN_POINT('',(0.,-3.25,0.));
#7731=CARTESIAN_POINT('',(0.,-0.45,-4.5));
#7732=CARTESIAN_POINT('',(0.,-2.,1.));
#7733=CARTESIAN_POINT('',(0.,32.,1.));
#7734=CARTESIAN_POINT('',(3.,0.45,4.5));
#7735=CARTESIAN_POINT('',(3.,0.45,4.5));
#7736=CARTESIAN_POINT('',(8.99785,0.45,4.5));
#7737=CARTESIAN_POINT('',(14.9957,0.45,4.5));
#7738=CARTESIAN_POINT('',(20.99355,0.45,4.5));
#7739=CARTESIAN_POINT('',(26.9914,0.45,4.5));
#7740=CARTESIAN_POINT('',(3.,0.,0.));
#7741=CARTESIAN_POINT('',(3.,0.,0.));
#7742=CARTESIAN_POINT('',(3.,30.,0.));
#7743=CARTESIAN_POINT('',(3.,0.,0.));
#7744=CARTESIAN_POINT('',(3.,30.3,0.));
#7745=CARTESIAN_POINT('',(4.9,-0.3,4.5));
#7746=CARTESIAN_POINT('',(3.,-0.3,6.4));
#7747=CARTESIAN_POINT('',(1.1,-0.3,4.5));
#7748=CARTESIAN_POINT('',(3.,-0.3,2.6));
#7749=CARTESIAN_POINT('',(4.9,30.3,4.5));
#7750=CARTESIAN_POINT('',(3.,30.3,6.4));
#7751=CARTESIAN_POINT('',(1.1,30.3,4.5));
#7752=CARTESIAN_POINT('',(3.,30.3,2.6));
#7753=CARTESIAN_POINT('',(0.,0.,0.));
#7754=CARTESIAN_POINT('',(3.61859725581877,0.,-0.872833278177676));
#7755=CARTESIAN_POINT('',(5.67817669064103,-3.5527136788005E-15,0.232039140127989));
#7756=CARTESIAN_POINT('',(13.9871309738653,3.5527136788005E-15,-0.81263553576726));
#7757=CARTESIAN_POINT('',(17.9629337384766,0.,0.0249325677576064));
#7758=CARTESIAN_POINT('',(24.4661966909013,-3.5527136788005E-15,-0.27805826573939));
#7759=UNCERTAINTY_MEASURE_WITH_UNIT(LENGTH_MEASURE(0.001),#7807,
'DISTANCE_ACCURACY_VALUE',
'Maximum model space distance between geometric entities at asserted c
onnectivities');
#7760=UNCERTAINTY_MEASURE_WITH_UNIT(LENGTH_MEASURE(0.001),#7807,
'DISTANCE_ACCURACY_VALUE',
'Maximum model space distance between geometric entities at asserted c
onnectivities');
#7761=UNCERTAINTY_MEASURE_WITH_UNIT(LENGTH_MEASURE(0.001),#7807,
'DISTANCE_ACCURACY_VALUE',
'Maximum model space distance between geometric entities at asserted c
onnectivities');
#7762=UNCERTAINTY_MEASURE_WITH_UNIT(LENGTH_MEASURE(0.001),#7807,
'DISTANCE_ACCURACY_VALUE',
'Maximum model space distance between geometric entities at asserted c
onnectivities');
#7763=UNCERTAINTY_MEASURE_WITH_UNIT(LENGTH_MEASURE(0.001),#7807,
'DISTANCE_ACCURACY_VALUE',
'Maximum model space distance between geometric entities at asserted c
onnectivities');
#7764=UNCERTAINTY_MEASURE_WITH_UNIT(LENGTH_MEASURE(0.001),#7807,
'DISTANCE_ACCURACY_VALUE',
'Maximum model space distance between geometric entities at asserted c
onnectivities');
#7765=UNCERTAINTY_MEASURE_WITH_UNIT(LENGTH_MEASURE(0.001),#7807,
'DISTANCE_ACCURACY_VALUE',
'Maximum model space distance between geometric entities at asserted c
onnectivities');
#7766=UNCERTAINTY_MEASURE_WITH_UNIT(LENGTH_MEASURE(0.001),#7807,
'DISTANCE_ACCURACY_VALUE',
'Maximum model space distance between geometric entities at asserted c
onnectivities');
#7767=UNCERTAINTY_MEASURE_WITH_UNIT(LENGTH_MEASURE(0.001),#7807,
'DISTANCE_ACCURACY_VALUE',
'Maximum model space distance between geometric entities at asserted c
onnectivities');
#7768=UNCERTAINTY_MEASURE_WITH_UNIT(LENGTH_MEASURE(0.001),#7807,
'DISTANCE_ACCURACY_VALUE',
'Maximum model space distance between geometric entities at asserted c
onnectivities');
#7769=UNCERTAINTY_MEASURE_WITH_UNIT(LENGTH_MEASURE(0.001),#7807,
'DISTANCE_ACCURACY_VALUE',
'Maximum model space distance between geometric entities at asserted c
onnectivities');
#7770=UNCERTAINTY_MEASURE_WITH_UNIT(LENGTH_MEASURE(0.001),#7807,
'DISTANCE_ACCURACY_VALUE',
'Maximum model space distance between geometric entities at asserted c
onnectivities');
#7771=UNCERTAINTY_MEASURE_WITH_UNIT(LENGTH_MEASURE(0.001),#7807,
'DISTANCE_ACCURACY_VALUE',
'Maximum model space distance between geometric entities at asserted c
onnectivities');
#7772=UNCERTAINTY_MEASURE_WITH_UNIT(LENGTH_MEASURE(0.001),#7807,
'DISTANCE_ACCURACY_VALUE',
'Maximum model space distance between geometric entities at asserted c
onnectivities');
#7773=UNCERTAINTY_MEASURE_WITH_UNIT(LENGTH_MEASURE(0.001),#7807,
'DISTANCE_ACCURACY_VALUE',
'Maximum model space distance between geometric entities at asserted c
onnectivities');
#7774=UNCERTAINTY_MEASURE_WITH_UNIT(LENGTH_MEASURE(0.001),#7807,
'DISTANCE_ACCURACY_VALUE',
'Maximum model space distance between geometric entities at asserted c
onnectivities');
#7775=UNCERTAINTY_MEASURE_WITH_UNIT(LENGTH_MEASURE(0.001),#7807,
'DISTANCE_ACCURACY_VALUE',
'Maximum model space distance between geometric entities at asserted c
onnectivities');
#7776=UNCERTAINTY_MEASURE_WITH_UNIT(LENGTH_MEASURE(0.001),#7807,
'DISTANCE_ACCURACY_VALUE',
'Maximum model space distance between geometric entities at asserted c
onnectivities');
#7777=UNCERTAINTY_MEASURE_WITH_UNIT(LENGTH_MEASURE(0.001),#7807,
'DISTANCE_ACCURACY_VALUE',
'Maximum model space distance between geometric entities at asserted c
onnectivities');
#7778=UNCERTAINTY_MEASURE_WITH_UNIT(LENGTH_MEASURE(0.001),#7807,
'DISTANCE_ACCURACY_VALUE',
'Maximum model space distance between geometric entities at asserted c
onnectivities');
#7779=UNCERTAINTY_MEASURE_WITH_UNIT(LENGTH_MEASURE(0.001),#7807,
'DISTANCE_ACCURACY_VALUE',
'Maximum model space distance between geometric entities at asserted c
onnectivities');
#7780=UNCERTAINTY_MEASURE_WITH_UNIT(LENGTH_MEASURE(0.001),#7807,
'DISTANCE_ACCURACY_VALUE',
'Maximum model space distance between geometric entities at asserted c
onnectivities');
#7781=UNCERTAINTY_MEASURE_WITH_UNIT(LENGTH_MEASURE(0.001),#7807,
'DISTANCE_ACCURACY_VALUE',
'Maximum model space distance between geometric entities at asserted c
onnectivities');
#7782=UNCERTAINTY_MEASURE_WITH_UNIT(LENGTH_MEASURE(0.001),#7807,
'DISTANCE_ACCURACY_VALUE',
'Maximum model space distance between geometric entities at asserted c
onnectivities');
#7783=(
GEOMETRIC_REPRESENTATION_CONTEXT(3)
GLOBAL_UNCERTAINTY_ASSIGNED_CONTEXT((#7759))
GLOBAL_UNIT_ASSIGNED_CONTEXT((#7807,#7809,#7810))
REPRESENTATION_CONTEXT('','3D')
);
#7784=(
GEOMETRIC_REPRESENTATION_CONTEXT(3)
GLOBAL_UNCERTAINTY_ASSIGNED_CONTEXT((#7760))
GLOBAL_UNIT_ASSIGNED_CONTEXT((#7807,#7809,#7810))
REPRESENTATION_CONTEXT('','3D')
);
#7785=(
GEOMETRIC_REPRESENTATION_CONTEXT(3)
GLOBAL_UNCERTAINTY_ASSIGNED_CONTEXT((#7761))
GLOBAL_UNIT_ASSIGNED_CONTEXT((#7807,#7809,#7810))
REPRESENTATION_CONTEXT('','3D')
);
#7786=(
GEOMETRIC_REPRESENTATION_CONTEXT(3)
GLOBAL_UNCERTAINTY_ASSIGNED_CONTEXT((#7762))
GLOBAL_UNIT_ASSIGNED_CONTEXT((#7807,#7809,#7810))
REPRESENTATION_CONTEXT('','3D')
);
#7787=(
GEOMETRIC_REPRESENTATION_CONTEXT(3)
GLOBAL_UNCERTAINTY_ASSIGNED_CONTEXT((#7763))
GLOBAL_UNIT_ASSIGNED_CONTEXT((#7807,#7809,#7810))
REPRESENTATION_CONTEXT('','3D')
);
#7788=(
GEOMETRIC_REPRESENTATION_CONTEXT(3)
GLOBAL_UNCERTAINTY_ASSIGNED_CONTEXT((#7764))
GLOBAL_UNIT_ASSIGNED_CONTEXT((#7807,#7809,#7810))
REPRESENTATION_CONTEXT('','3D')
);
#7789=(
GEOMETRIC_REPRESENTATION_CONTEXT(3)
GLOBAL_UNCERTAINTY_ASSIGNED_CONTEXT((#7765))
GLOBAL_UNIT_ASSIGNED_CONTEXT((#7807,#7809,#7810))
REPRESENTATION_CONTEXT('','3D')
);
#7790=(
GEOMETRIC_REPRESENTATION_CONTEXT(3)
GLOBAL_UNCERTAINTY_ASSIGNED_CONTEXT((#7766))
GLOBAL_UNIT_ASSIGNED_CONTEXT((#7807,#7809,#7810))
REPRESENTATION_CONTEXT('','3D')
);
#7791=(
GEOMETRIC_REPRESENTATION_CONTEXT(3)
GLOBAL_UNCERTAINTY_ASSIGNED_CONTEXT((#7767))
GLOBAL_UNIT_ASSIGNED_CONTEXT((#7807,#7809,#7810))
REPRESENTATION_CONTEXT('','3D')
);
#7792=(
GEOMETRIC_REPRESENTATION_CONTEXT(3)
GLOBAL_UNCERTAINTY_ASSIGNED_CONTEXT((#7768))
GLOBAL_UNIT_ASSIGNED_CONTEXT((#7807,#7809,#7810))
REPRESENTATION_CONTEXT('','3D')
);
#7793=(
GEOMETRIC_REPRESENTATION_CONTEXT(3)
GLOBAL_UNCERTAINTY_ASSIGNED_CONTEXT((#7769))
GLOBAL_UNIT_ASSIGNED_CONTEXT((#7807,#7809,#7810))
REPRESENTATION_CONTEXT('','3D')
);
#7794=(
GEOMETRIC_REPRESENTATION_CONTEXT(3)
GLOBAL_UNCERTAINTY_ASSIGNED_CONTEXT((#7770))
GLOBAL_UNIT_ASSIGNED_CONTEXT((#7807,#7809,#7810))
REPRESENTATION_CONTEXT('','3D')
);
#7795=(
GEOMETRIC_REPRESENTATION_CONTEXT(3)
GLOBAL_UNCERTAINTY_ASSIGNED_CONTEXT((#7771))
GLOBAL_UNIT_ASSIGNED_CONTEXT((#7807,#7809,#7810))
REPRESENTATION_CONTEXT('','3D')
);
#7796=(
GEOMETRIC_REPRESENTATION_CONTEXT(3)
GLOBAL_UNCERTAINTY_ASSIGNED_CONTEXT((#7772))
GLOBAL_UNIT_ASSIGNED_CONTEXT((#7807,#7809,#7810))
REPRESENTATION_CONTEXT('','3D')
);
#7797=(
GEOMETRIC_REPRESENTATION_CONTEXT(3)
GLOBAL_UNCERTAINTY_ASSIGNED_CONTEXT((#7773))
GLOBAL_UNIT_ASSIGNED_CONTEXT((#7807,#7809,#7810))
REPRESENTATION_CONTEXT('','3D')
);
#7798=(
GEOMETRIC_REPRESENTATION_CONTEXT(3)
GLOBAL_UNCERTAINTY_ASSIGNED_CONTEXT((#7774))
GLOBAL_UNIT_ASSIGNED_CONTEXT((#7807,#7809,#7810))
REPRESENTATION_CONTEXT('','3D')
);
#7799=(
GEOMETRIC_REPRESENTATION_CONTEXT(3)
GLOBAL_UNCERTAINTY_ASSIGNED_CONTEXT((#7775))
GLOBAL_UNIT_ASSIGNED_CONTEXT((#7807,#7809,#7810))
REPRESENTATION_CONTEXT('','3D')
);
#7800=(
GEOMETRIC_REPRESENTATION_CONTEXT(3)
GLOBAL_UNCERTAINTY_ASSIGNED_CONTEXT((#7776))
GLOBAL_UNIT_ASSIGNED_CONTEXT((#7807,#7809,#7810))
REPRESENTATION_CONTEXT('','3D')
);
#7801=(
GEOMETRIC_REPRESENTATION_CONTEXT(3)
GLOBAL_UNCERTAINTY_ASSIGNED_CONTEXT((#7777))
GLOBAL_UNIT_ASSIGNED_CONTEXT((#7807,#7809,#7810))
REPRESENTATION_CONTEXT('','3D')
);
#7802=(
GEOMETRIC_REPRESENTATION_CONTEXT(3)
GLOBAL_UNCERTAINTY_ASSIGNED_CONTEXT((#7778))
GLOBAL_UNIT_ASSIGNED_CONTEXT((#7807,#7809,#7810))
REPRESENTATION_CONTEXT('','3D')
);
#7803=(
GEOMETRIC_REPRESENTATION_CONTEXT(3)
GLOBAL_UNCERTAINTY_ASSIGNED_CONTEXT((#7779))
GLOBAL_UNIT_ASSIGNED_CONTEXT((#7807,#7809,#7810))
REPRESENTATION_CONTEXT('','3D')
);
#7804=(
GEOMETRIC_REPRESENTATION_CONTEXT(3)
GLOBAL_UNCERTAINTY_ASSIGNED_CONTEXT((#7780))
GLOBAL_UNIT_ASSIGNED_CONTEXT((#7807,#7809,#7810))
REPRESENTATION_CONTEXT('','3D')
);
#7805=(
GEOMETRIC_REPRESENTATION_CONTEXT(3)
GLOBAL_UNCERTAINTY_ASSIGNED_CONTEXT((#7781))
GLOBAL_UNIT_ASSIGNED_CONTEXT((#7807,#7809,#7810))
REPRESENTATION_CONTEXT('','3D')
);
#7806=(
GEOMETRIC_REPRESENTATION_CONTEXT(3)
GLOBAL_UNCERTAINTY_ASSIGNED_CONTEXT((#7782))
GLOBAL_UNIT_ASSIGNED_CONTEXT((#7807,#7809,#7810))
REPRESENTATION_CONTEXT('','3D')
);
#7807=(
LENGTH_UNIT()
NAMED_UNIT(*)
SI_UNIT(.CENTI.,.METRE.)
);
#7808=(
LENGTH_UNIT()
NAMED_UNIT(*)
SI_UNIT($,.METRE.)
);
#7809=(
NAMED_UNIT(*)
PLANE_ANGLE_UNIT()
SI_UNIT($,.RADIAN.)
);
#7810=(
NAMED_UNIT(*)
SI_UNIT($,.STERADIAN.)
SOLID_ANGLE_UNIT()
);
#7811=SHAPE_DEFINITION_REPRESENTATION(#7834,#7910);
#7812=SHAPE_DEFINITION_REPRESENTATION(#7835,#7911);
#7813=SHAPE_DEFINITION_REPRESENTATION(#7836,#7912);
#7814=SHAPE_DEFINITION_REPRESENTATION(#7837,#7913);
#7815=SHAPE_DEFINITION_REPRESENTATION(#7838,#7914);
#7816=SHAPE_DEFINITION_REPRESENTATION(#7839,#7915);
#7817=SHAPE_DEFINITION_REPRESENTATION(#7840,#7916);
#7818=SHAPE_DEFINITION_REPRESENTATION(#7841,#7917);
#7819=SHAPE_DEFINITION_REPRESENTATION(#7842,#7918);
#7820=SHAPE_DEFINITION_REPRESENTATION(#7843,#7919);
#7821=SHAPE_DEFINITION_REPRESENTATION(#7844,#7920);
#7822=SHAPE_DEFINITION_REPRESENTATION(#7845,#7921);
#7823=SHAPE_DEFINITION_REPRESENTATION(#7846,#7922);
#7824=SHAPE_DEFINITION_REPRESENTATION(#7847,#7923);
#7825=SHAPE_DEFINITION_REPRESENTATION(#7848,#7924);
#7826=SHAPE_DEFINITION_REPRESENTATION(#7854,#7925);
#7827=SHAPE_DEFINITION_REPRESENTATION(#7855,#7926);
#7828=SHAPE_DEFINITION_REPRESENTATION(#7856,#7927);
#7829=SHAPE_DEFINITION_REPRESENTATION(#7857,#7928);
#7830=SHAPE_DEFINITION_REPRESENTATION(#7858,#7929);
#7831=SHAPE_DEFINITION_REPRESENTATION(#7859,#7930);
#7832=SHAPE_DEFINITION_REPRESENTATION(#7860,#7931);
#7833=SHAPE_DEFINITION_REPRESENTATION(#7861,#7932);
#7834=PRODUCT_DEFINITION_SHAPE('',$,#7934);
#7835=PRODUCT_DEFINITION_SHAPE('',$,#7935);
#7836=PRODUCT_DEFINITION_SHAPE('',$,#7936);
#7837=PRODUCT_DEFINITION_SHAPE('',$,#7937);
#7838=PRODUCT_DEFINITION_SHAPE('',$,#7938);
#7839=PRODUCT_DEFINITION_SHAPE('',$,#7939);
#7840=PRODUCT_DEFINITION_SHAPE('',$,#7940);
#7841=PRODUCT_DEFINITION_SHAPE('',$,#7941);
#7842=PRODUCT_DEFINITION_SHAPE('',$,#7942);
#7843=PRODUCT_DEFINITION_SHAPE('',$,#7943);
#7844=PRODUCT_DEFINITION_SHAPE('',$,#7944);
#7845=PRODUCT_DEFINITION_SHAPE('',$,#7945);
#7846=PRODUCT_DEFINITION_SHAPE('',$,#7946);
#7847=PRODUCT_DEFINITION_SHAPE('',$,#7947);
#7848=PRODUCT_DEFINITION_SHAPE('',$,#7948);
#7849=PRODUCT_DEFINITION_SHAPE($,$,#170);
#7850=PRODUCT_DEFINITION_SHAPE($,$,#171);
#7851=PRODUCT_DEFINITION_SHAPE($,$,#172);
#7852=PRODUCT_DEFINITION_SHAPE($,$,#173);
#7853=PRODUCT_DEFINITION_SHAPE($,$,#174);
#7854=PRODUCT_DEFINITION_SHAPE('',$,#7949);
#7855=PRODUCT_DEFINITION_SHAPE('',$,#7950);
#7856=PRODUCT_DEFINITION_SHAPE('',$,#7951);
#7857=PRODUCT_DEFINITION_SHAPE('',$,#7952);
#7858=PRODUCT_DEFINITION_SHAPE('',$,#7953);
#7859=PRODUCT_DEFINITION_SHAPE('',$,#7954);
#7860=PRODUCT_DEFINITION_SHAPE('',$,#7955);
#7861=PRODUCT_DEFINITION_SHAPE('',$,#7956);
#7862=PRODUCT_DEFINITION_SHAPE($,$,#175);
#7863=PRODUCT_DEFINITION_SHAPE($,$,#176);
#7864=PRODUCT_DEFINITION_SHAPE($,$,#177);
#7865=PRODUCT_DEFINITION_SHAPE($,$,#178);
#7866=PRODUCT_DEFINITION_SHAPE($,$,#179);
#7867=PRODUCT_DEFINITION_SHAPE($,$,#180);
#7868=PRODUCT_DEFINITION_SHAPE($,$,#181);
#7869=PRODUCT_DEFINITION_SHAPE($,$,#182);
#7870=PRODUCT_DEFINITION_SHAPE($,$,#183);
#7871=PRODUCT_DEFINITION_SHAPE($,$,#184);
#7872=PRODUCT_DEFINITION_SHAPE($,$,#185);
#7873=PRODUCT_DEFINITION_SHAPE($,$,#186);
#7874=PRODUCT_DEFINITION_SHAPE($,$,#187);
#7875=PRODUCT_DEFINITION_SHAPE($,$,#188);
#7876=PRODUCT_DEFINITION_SHAPE($,$,#189);
#7877=PRODUCT_DEFINITION_SHAPE($,$,#190);
#7878=PRODUCT_DEFINITION_SHAPE($,$,#191);
#7879=PRODUCT_DEFINITION_SHAPE($,$,#192);
#7880=PRODUCT_DEFINITION_SHAPE($,$,#193);
#7881=PRODUCT_DEFINITION_SHAPE($,$,#194);
#7882=PRODUCT_DEFINITION_SHAPE($,$,#195);
#7883=PRODUCT_DEFINITION_SHAPE($,$,#196);
#7884=PRODUCT_DEFINITION_SHAPE($,$,#197);
#7885=PRODUCT_DEFINITION_SHAPE($,$,#198);
#7886=PRODUCT_DEFINITION_SHAPE($,$,#199);
#7887=PRODUCT_DEFINITION_SHAPE($,$,#200);
#7888=PRODUCT_DEFINITION_SHAPE($,$,#201);
#7889=PRODUCT_DEFINITION_SHAPE($,$,#202);
#7890=PRODUCT_DEFINITION_SHAPE($,$,#203);
#7891=PRODUCT_DEFINITION_SHAPE($,$,#204);
#7892=PRODUCT_DEFINITION_SHAPE($,$,#205);
#7893=PRODUCT_DEFINITION_SHAPE($,$,#206);
#7894=PRODUCT_DEFINITION_SHAPE($,$,#207);
#7895=PRODUCT_DEFINITION_SHAPE($,$,#208);
#7896=PRODUCT_DEFINITION_SHAPE($,$,#209);
#7897=PRODUCT_DEFINITION_SHAPE($,$,#210);
#7898=PRODUCT_DEFINITION_SHAPE($,$,#211);
#7899=PRODUCT_DEFINITION_SHAPE($,$,#212);
#7900=PRODUCT_DEFINITION_SHAPE($,$,#213);
#7901=PRODUCT_DEFINITION_SHAPE($,$,#214);
#7902=PRODUCT_DEFINITION_SHAPE($,$,#215);
#7903=PRODUCT_DEFINITION_SHAPE($,$,#216);
#7904=PRODUCT_DEFINITION_SHAPE($,$,#217);
#7905=PRODUCT_DEFINITION_SHAPE($,$,#218);
#7906=PRODUCT_DEFINITION_SHAPE($,$,#219);
#7907=PRODUCT_DEFINITION_SHAPE($,$,#220);
#7908=PRODUCT_DEFINITION_SHAPE($,$,#221);
#7909=PRODUCT_DEFINITION_SHAPE($,$,#222);
#7910=SHAPE_REPRESENTATION('',(#4426,#4903,#4904,#4905,#4906,#4907,#4908),
#7783);
#7911=SHAPE_REPRESENTATION('',(#4427,#4882,#4883,#4884,#4885,#4886,#4887,
#4888,#4889),#7784);
#7912=SHAPE_REPRESENTATION('',(#4428),#7785);
#7913=SHAPE_REPRESENTATION('',(#4478,#4861,#4862,#4863,#4864,#4865,#4866,
#4867,#4868,#4869,#4870,#4871,#4872,#4873,#4874,#4875,#4876,#4877,#4878,
#4879,#4880,#4881),#7786);
#7914=SHAPE_REPRESENTATION('',(#4479),#7787);
#7915=SHAPE_REPRESENTATION('',(#4501),#7788);
#7916=SHAPE_REPRESENTATION('',(#4537),#7789);
#7917=SHAPE_REPRESENTATION('',(#4573),#7790);
#7918=SHAPE_REPRESENTATION('',(#4597),#7791);
#7919=SHAPE_REPRESENTATION('',(#4618,#4747,#4748,#4749,#4750,#4751),#7792);
#7920=SHAPE_REPRESENTATION('',(#4619),#7793);
#7921=SHAPE_REPRESENTATION('',(#4639),#7794);
#7922=SHAPE_REPRESENTATION('',(#4659),#7795);
#7923=SHAPE_REPRESENTATION('',(#4676),#7796);
#7924=SHAPE_REPRESENTATION('',(#4730),#7797);
#7925=SHAPE_REPRESENTATION('',(#4752),#7798);
#7926=SHAPE_REPRESENTATION('',(#4761),#7799);
#7927=SHAPE_REPRESENTATION('',(#4770),#7800);
#7928=SHAPE_REPRESENTATION('',(#4779,#4890,#4891,#4892,#4893,#4894,#4895,
#4896,#4897,#4898,#4899,#4900,#4901,#4902),#7801);
#7929=SHAPE_REPRESENTATION('',(#4780),#7802);
#7930=SHAPE_REPRESENTATION('',(#4789),#7803);
#7931=SHAPE_REPRESENTATION('',(#4814),#7804);
#7932=SHAPE_REPRESENTATION('',(#4835),#7805);
#7933=PRODUCT_DEFINITION_CONTEXT('part definition',#8004,'design');
#7934=PRODUCT_DEFINITION('PAT-035','PAT-035',#7957,
#7933);
#7935=PRODUCT_DEFINITION('Extrusion frame axles and bearings',
'Extrusion frame axles and bearings',#7958,#7933);
#7936=PRODUCT_DEFINITION('Slotted Extrusion - 20 x 20 x 300 mm',
'Slotted Extrusion - 20 x 20 x 300 mm',#7959,#7933);
#7937=PRODUCT_DEFINITION('Axle Assembly','Axle Assembly',#7960,
#7933);
#7938=PRODUCT_DEFINITION('Axle','Axle',#7961,#7933);
#7939=PRODUCT_DEFINITION('Axle Mount A','Axle Mount A',#7962,#7933);
#7940=PRODUCT_DEFINITION('Axle Mount B','Axle Mount B',#7963,#7933);
#7941=PRODUCT_DEFINITION('M5x14 Cap Screw','M5x14 Cap Screw',#7964,#7933);
#7942=PRODUCT_DEFINITION('Slot nut','Slot nut',#7965,#7933);
#7943=PRODUCT_DEFINITION('Bearing','Bearing',#7966,#7933);
#7944=PRODUCT_DEFINITION('Inner ring','Inner ring',#7967,#7933);
#7945=PRODUCT_DEFINITION('Outer ring','Outer ring',#7968,#7933);
#7946=PRODUCT_DEFINITION('Balls','Balls',#7969,#7933);
#7947=PRODUCT_DEFINITION('Cage','Cage',#7970,#7933);
#7948=PRODUCT_DEFINITION('Seals 2RS','Seals 2RS',#7971,#7933);
#7949=PRODUCT_DEFINITION('End keeper','End keeper',#7972,#7933);
#7950=PRODUCT_DEFINITION('Spacer','Spacer',#7973,#7933);
#7951=PRODUCT_DEFINITION('Bracket spacer','Bracket spacer',#7974,#7933);
#7952=PRODUCT_DEFINITION('Roller Assembly','Roller Assembly',#7975,#7933);
#7953=PRODUCT_DEFINITION('Roller tube','Roller tube',#7976,#7933);
#7954=PRODUCT_DEFINITION('Bearing insert','Bearing insert',#7977,#7933);
#7955=PRODUCT_DEFINITION('Outer race retainer','Outer race retainer',#7978,
#7933);
#7956=PRODUCT_DEFINITION('Cap Screw - M4x16','Cap Screw - M4x16',#7979,
#7933);
#7957=PRODUCT_DEFINITION_FORMATION('',$,#8006);
#7958=PRODUCT_DEFINITION_FORMATION('',$,#8007);
#7959=PRODUCT_DEFINITION_FORMATION('',$,#8008);
#7960=PRODUCT_DEFINITION_FORMATION('',$,#8009);
#7961=PRODUCT_DEFINITION_FORMATION('',$,#8010);
#7962=PRODUCT_DEFINITION_FORMATION('',$,#8011);
#7963=PRODUCT_DEFINITION_FORMATION('',$,#8012);
#7964=PRODUCT_DEFINITION_FORMATION('',$,#8013);
#7965=PRODUCT_DEFINITION_FORMATION('',$,#8014);
#7966=PRODUCT_DEFINITION_FORMATION('',$,#8015);
#7967=PRODUCT_DEFINITION_FORMATION('',$,#8016);
#7968=PRODUCT_DEFINITION_FORMATION('',$,#8017);
#7969=PRODUCT_DEFINITION_FORMATION('',$,#8018);
#7970=PRODUCT_DEFINITION_FORMATION('',$,#8019);
#7971=PRODUCT_DEFINITION_FORMATION('',$,#8020);
#7972=PRODUCT_DEFINITION_FORMATION('',$,#8021);
#7973=PRODUCT_DEFINITION_FORMATION('',$,#8022);
#7974=PRODUCT_DEFINITION_FORMATION('',$,#8023);
#7975=PRODUCT_DEFINITION_FORMATION('',$,#8024);
#7976=PRODUCT_DEFINITION_FORMATION('',$,#8025);
#7977=PRODUCT_DEFINITION_FORMATION('',$,#8026);
#7978=PRODUCT_DEFINITION_FORMATION('',$,#8027);
#7979=PRODUCT_DEFINITION_FORMATION('',$,#8028);
#7980=PRODUCT_RELATED_PRODUCT_CATEGORY('PAT-035','PAT-035',(#8006));
#7981=PRODUCT_RELATED_PRODUCT_CATEGORY(
'Extrusion frame axles and bearings',
'Extrusion frame axles and bearings',(#8007));
#7982=PRODUCT_RELATED_PRODUCT_CATEGORY(
'Slotted Extrusion - 20 x 20 x 300 mm',
'Slotted Extrusion - 20 x 20 x 300 mm',(#8008));
#7983=PRODUCT_RELATED_PRODUCT_CATEGORY('Axle Assembly','Axle Assembly',
(#8009));
#7984=PRODUCT_RELATED_PRODUCT_CATEGORY('Axle','Axle',(#8010));
#7985=PRODUCT_RELATED_PRODUCT_CATEGORY('Axle Mount A','Axle Mount A',(#8011));
#7986=PRODUCT_RELATED_PRODUCT_CATEGORY('Axle Mount B','Axle Mount B',(#8012));
#7987=PRODUCT_RELATED_PRODUCT_CATEGORY('M5x14 Cap Screw',
'M5x14 Cap Screw',(#8013));
#7988=PRODUCT_RELATED_PRODUCT_CATEGORY('Slot nut','Slot nut',(#8014));
#7989=PRODUCT_RELATED_PRODUCT_CATEGORY('Bearing','Bearing',(#8015));
#7990=PRODUCT_RELATED_PRODUCT_CATEGORY('Inner ring','Inner ring',(#8016));
#7991=PRODUCT_RELATED_PRODUCT_CATEGORY('Outer ring','Outer ring',(#8017));
#7992=PRODUCT_RELATED_PRODUCT_CATEGORY('Balls','Balls',(#8018));
#7993=PRODUCT_RELATED_PRODUCT_CATEGORY('Cage','Cage',(#8019));
#7994=PRODUCT_RELATED_PRODUCT_CATEGORY('Seals 2RS','Seals 2RS',(#8020));
#7995=PRODUCT_RELATED_PRODUCT_CATEGORY('End keeper','End keeper',(#8021));
#7996=PRODUCT_RELATED_PRODUCT_CATEGORY('Spacer','Spacer',(#8022));
#7997=PRODUCT_RELATED_PRODUCT_CATEGORY('Bracket spacer',
'Bracket spacer',(#8023));
#7998=PRODUCT_RELATED_PRODUCT_CATEGORY('Roller Assembly',
'Roller Assembly',(#8024));
#7999=PRODUCT_RELATED_PRODUCT_CATEGORY('Roller tube','Roller tube',(#8025));
#8000=PRODUCT_RELATED_PRODUCT_CATEGORY('Bearing insert',
'Bearing insert',(#8026));
#8001=PRODUCT_RELATED_PRODUCT_CATEGORY('Outer race retainer',
'Outer race retainer',(#8027));
#8002=PRODUCT_RELATED_PRODUCT_CATEGORY('Cap Screw - M4x16',
'Cap Screw - M4x16',(#8028));
#8003=APPLICATION_PROTOCOL_DEFINITION('international standard',
'automotive_design',2009,#8004);
#8004=APPLICATION_CONTEXT(
'Core Data for Automotive Mechanical Design Process');
#8005=PRODUCT_CONTEXT('part definition',#8004,'mechanical');
#8006=PRODUCT('PAT-035','PAT-035',
'PAT-035',(#8005));
#8007=PRODUCT('Extrusion frame axles and bearings',
'Extrusion frame axles and bearings',
'Extrusion frame axles and bearings',(#8005));
#8008=PRODUCT('Slotted Extrusion - 20 x 20 x 300 mm',
'Slotted Extrusion - 20 x 20 x 300 mm',
'Slotted Extrusion - 20 x 20 x 300 mm',(#8005));
#8009=PRODUCT('Axle Assembly','Axle Assembly','Axle Assembly',(#8005));
#8010=PRODUCT('Axle','Axle','Axle',(#8005));
#8011=PRODUCT('Axle Mount A','Axle Mount A','Axle Mount A',(#8005));
#8012=PRODUCT('Axle Mount B','Axle Mount B','Axle Mount B',
(#8005));
#8013=PRODUCT('M5x14 Cap Screw','M5x14 Cap Screw','M5x14 Cap Screw',(#8005));
#8014=PRODUCT('Slot nut','Slot nut','Slot nut',(#8005));
#8015=PRODUCT('Bearing','Bearing',
'Bearing',(#8005));
#8016=PRODUCT('Inner ring','Inner ring','Inner ring',(#8005));
#8017=PRODUCT('Outer ring','Outer ring','Outer ring',(#8005));
#8018=PRODUCT('Balls','Balls','Balls',(#8005));
#8019=PRODUCT('Cage','Cage','Cage',(#8005));
#8020=PRODUCT('Seals 2RS','Seals 2RS','Seals 2RS',(#8005));
#8021=PRODUCT('End keeper','End keeper','End keeper',(#8005));
#8022=PRODUCT('Spacer','Spacer','Spacer',(#8005));
#8023=PRODUCT('Bracket spacer','Bracket spacer','Bracket spacer',(#8005));
#8024=PRODUCT('Roller Assembly','Roller Assembly','Roller Assembly',(#8005));
#8025=PRODUCT('Roller tube','Roller tube','Roller tube',(#8005));
#8026=PRODUCT('Bearing insert','Bearing insert','Bearing insert',(#8005));
#8027=PRODUCT('Outer race retainer','Outer race retainer',
'Outer race retainer',(#8005));
#8028=PRODUCT('Cap Screw - M4x16','Cap Screw - M4x16',
'Cap Screw - M4x16',(#8005));
#8029=PRESENTATION_STYLE_ASSIGNMENT((#8034));
#8030=PRESENTATION_STYLE_ASSIGNMENT((#8035));
#8031=PRESENTATION_STYLE_ASSIGNMENT((#8036));
#8032=PRESENTATION_STYLE_ASSIGNMENT((#8037));
#8033=PRESENTATION_STYLE_ASSIGNMENT((#8038));
#8034=SURFACE_STYLE_USAGE(.BOTH.,#8039);
#8035=SURFACE_STYLE_USAGE(.BOTH.,#8040);
#8036=SURFACE_STYLE_USAGE(.BOTH.,#8041);
#8037=SURFACE_STYLE_USAGE(.BOTH.,#8042);
#8038=SURFACE_STYLE_USAGE(.BOTH.,#8043);
#8039=SURFACE_SIDE_STYLE('',(#8044));
#8040=SURFACE_SIDE_STYLE('',(#8045));
#8041=SURFACE_SIDE_STYLE('',(#8046));
#8042=SURFACE_SIDE_STYLE('',(#8047));
#8043=SURFACE_SIDE_STYLE('',(#8048));
#8044=SURFACE_STYLE_FILL_AREA(#8049);
#8045=SURFACE_STYLE_FILL_AREA(#8050);
#8046=SURFACE_STYLE_FILL_AREA(#8051);
#8047=SURFACE_STYLE_FILL_AREA(#8052);
#8048=SURFACE_STYLE_FILL_AREA(#8053);
#8049=FILL_AREA_STYLE('Steel - Satin',(#8054));
#8050=FILL_AREA_STYLE('CAD Library Painted - Steel gray',(#8055));
#8051=FILL_AREA_STYLE('CAD Library Painted - Engineering blue',(#8056));
#8052=FILL_AREA_STYLE('CAD Library Painted - Graphite',(#8057));
#8053=FILL_AREA_STYLE('CAD Library Painted - Off white',(#8058));
#8054=FILL_AREA_STYLE_COLOUR('Steel - Satin',#8059);
#8055=FILL_AREA_STYLE_COLOUR('CAD Library Painted - Steel gray',#8060);
#8056=FILL_AREA_STYLE_COLOUR('CAD Library Painted - Engineering blue',#8061);
#8057=FILL_AREA_STYLE_COLOUR('CAD Library Painted - Graphite',#8062);
#8058=FILL_AREA_STYLE_COLOUR('CAD Library Painted - Off white',#8063);
#8059=COLOUR_RGB('Steel - Satin',0.627450980392157,0.627450980392157,0.627450980392157);
#8060=COLOUR_RGB('CAD Library Painted - Steel gray',0.592156862745098,0.631372549019608,
0.67843137254902);
#8061=COLOUR_RGB('CAD Library Painted - Engineering blue',0.12156862745098,
0.356862745098039,0.6);
#8062=COLOUR_RGB('CAD Library Painted - Graphite',0.0980392156862745,0.109803921568627,
0.125490196078431);
#8063=COLOUR_RGB('CAD Library Painted - Off white',0.909803921568627,0.901960784313726,
0.858823529411765);
#8064=COLOUR_RGB('Dark Blue',0.08,0.2,0.34);
#8065=FILL_AREA_STYLE_COLOUR('',#8064);
#8066=FILL_AREA_STYLE('',(#8065));
#8067=SURFACE_STYLE_FILL_AREA(#8066);
#8068=SURFACE_SIDE_STYLE('',(#8067));
#8069=SURFACE_STYLE_USAGE(.BOTH.,#8068);
#8070=PRESENTATION_STYLE_ASSIGNMENT((#8069));
#8071=COLOUR_RGB('Light Blue',0.38,0.62,0.78);
#8072=FILL_AREA_STYLE_COLOUR('',#8071);
#8073=FILL_AREA_STYLE('',(#8072));
#8074=SURFACE_STYLE_FILL_AREA(#8073);
#8075=SURFACE_SIDE_STYLE('',(#8074));
#8076=SURFACE_STYLE_USAGE(.BOTH.,#8075);
#8077=PRESENTATION_STYLE_ASSIGNMENT((#8076));
#8078=COLOUR_RGB('Sky Blue',0.24,0.69,0.87);
#8079=FILL_AREA_STYLE_COLOUR('',#8078);
#8080=FILL_AREA_STYLE('',(#8079));
#8081=SURFACE_STYLE_FILL_AREA(#8080);
#8082=SURFACE_SIDE_STYLE('',(#8081));
#8083=SURFACE_STYLE_USAGE(.BOTH.,#8082);
#8084=PRESENTATION_STYLE_ASSIGNMENT((#8083));
#8085=COLOUR_RGB('Grey',0.48,0.52,0.57);
#8086=FILL_AREA_STYLE_COLOUR('',#8085);
#8087=FILL_AREA_STYLE('',(#8086));
#8088=SURFACE_STYLE_FILL_AREA(#8087);
#8089=SURFACE_SIDE_STYLE('',(#8088));
#8090=SURFACE_STYLE_USAGE(.BOTH.,#8089);
#8091=PRESENTATION_STYLE_ASSIGNMENT((#8090));
#8092=COLOUR_RGB('Black',0.12,0.14,0.17);
#8093=FILL_AREA_STYLE_COLOUR('',#8092);
#8094=FILL_AREA_STYLE('',(#8093));
#8095=SURFACE_STYLE_FILL_AREA(#8094);
#8096=SURFACE_SIDE_STYLE('',(#8095));
#8097=SURFACE_STYLE_USAGE(.BOTH.,#8096);
#8098=PRESENTATION_STYLE_ASSIGNMENT((#8097));
#8099=COLOUR_RGB('Off White',0.89,0.88,0.83);
#8100=FILL_AREA_STYLE_COLOUR('',#8099);
#8101=FILL_AREA_STYLE('',(#8100));
#8102=SURFACE_STYLE_FILL_AREA(#8101);
#8103=SURFACE_SIDE_STYLE('',(#8102));
#8104=SURFACE_STYLE_USAGE(.BOTH.,#8103);
#8105=PRESENTATION_STYLE_ASSIGNMENT((#8104));
ENDSEC;
END-ISO-10303-21;
